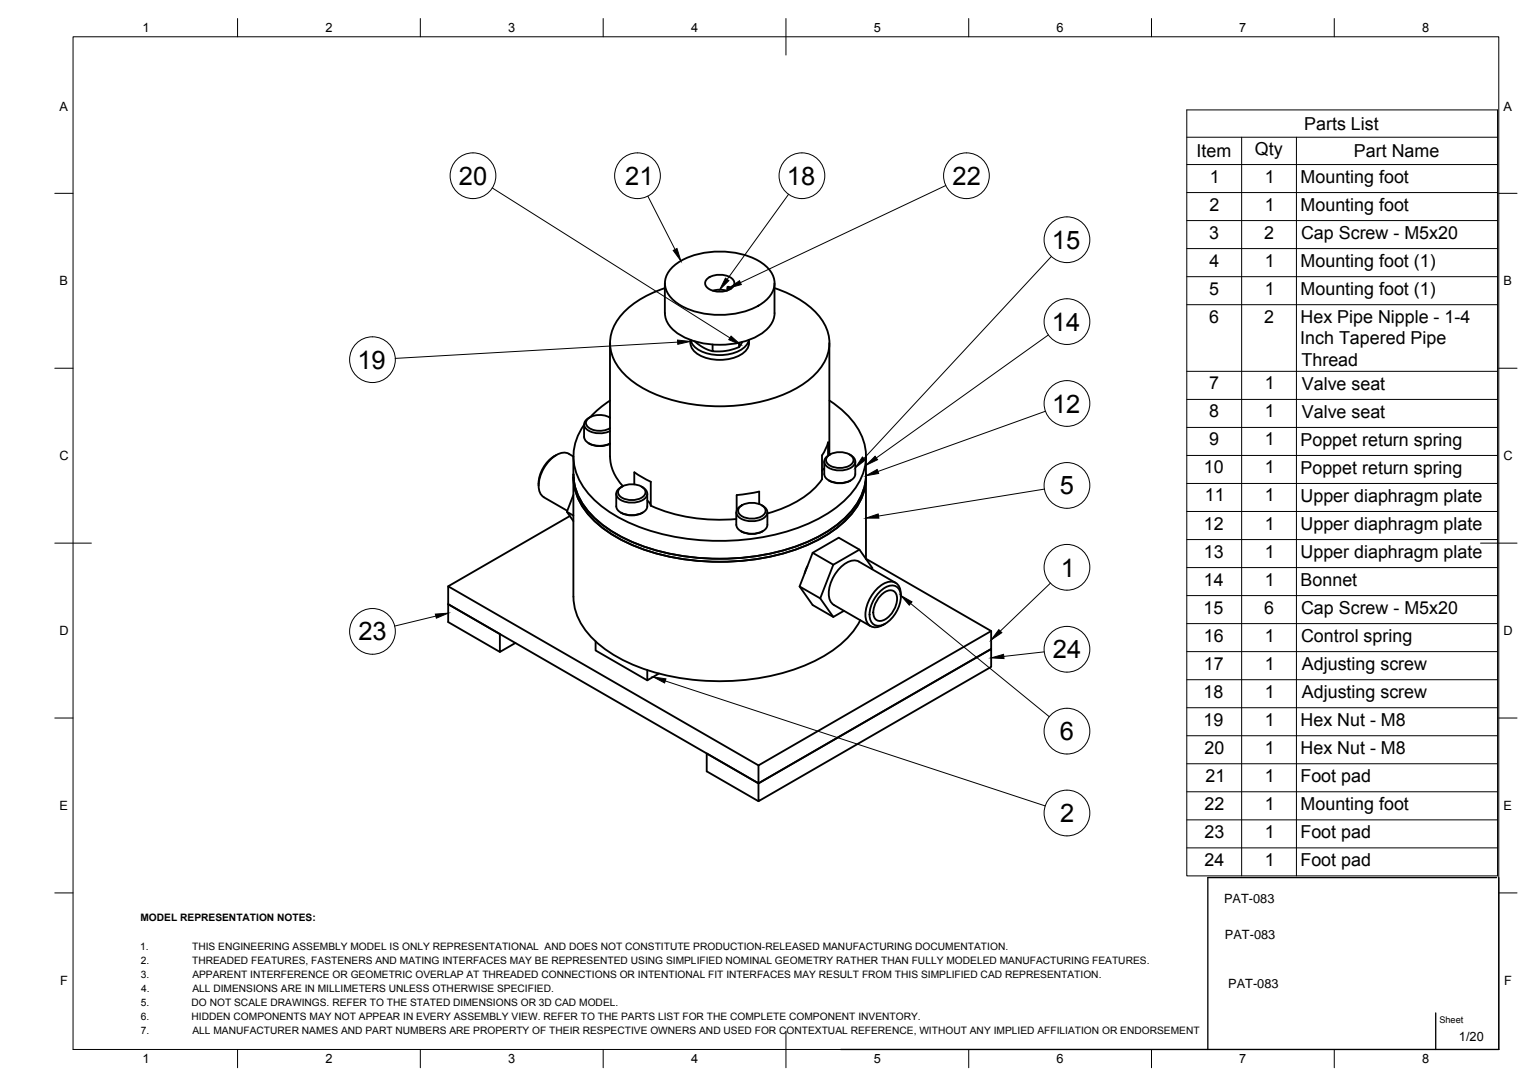
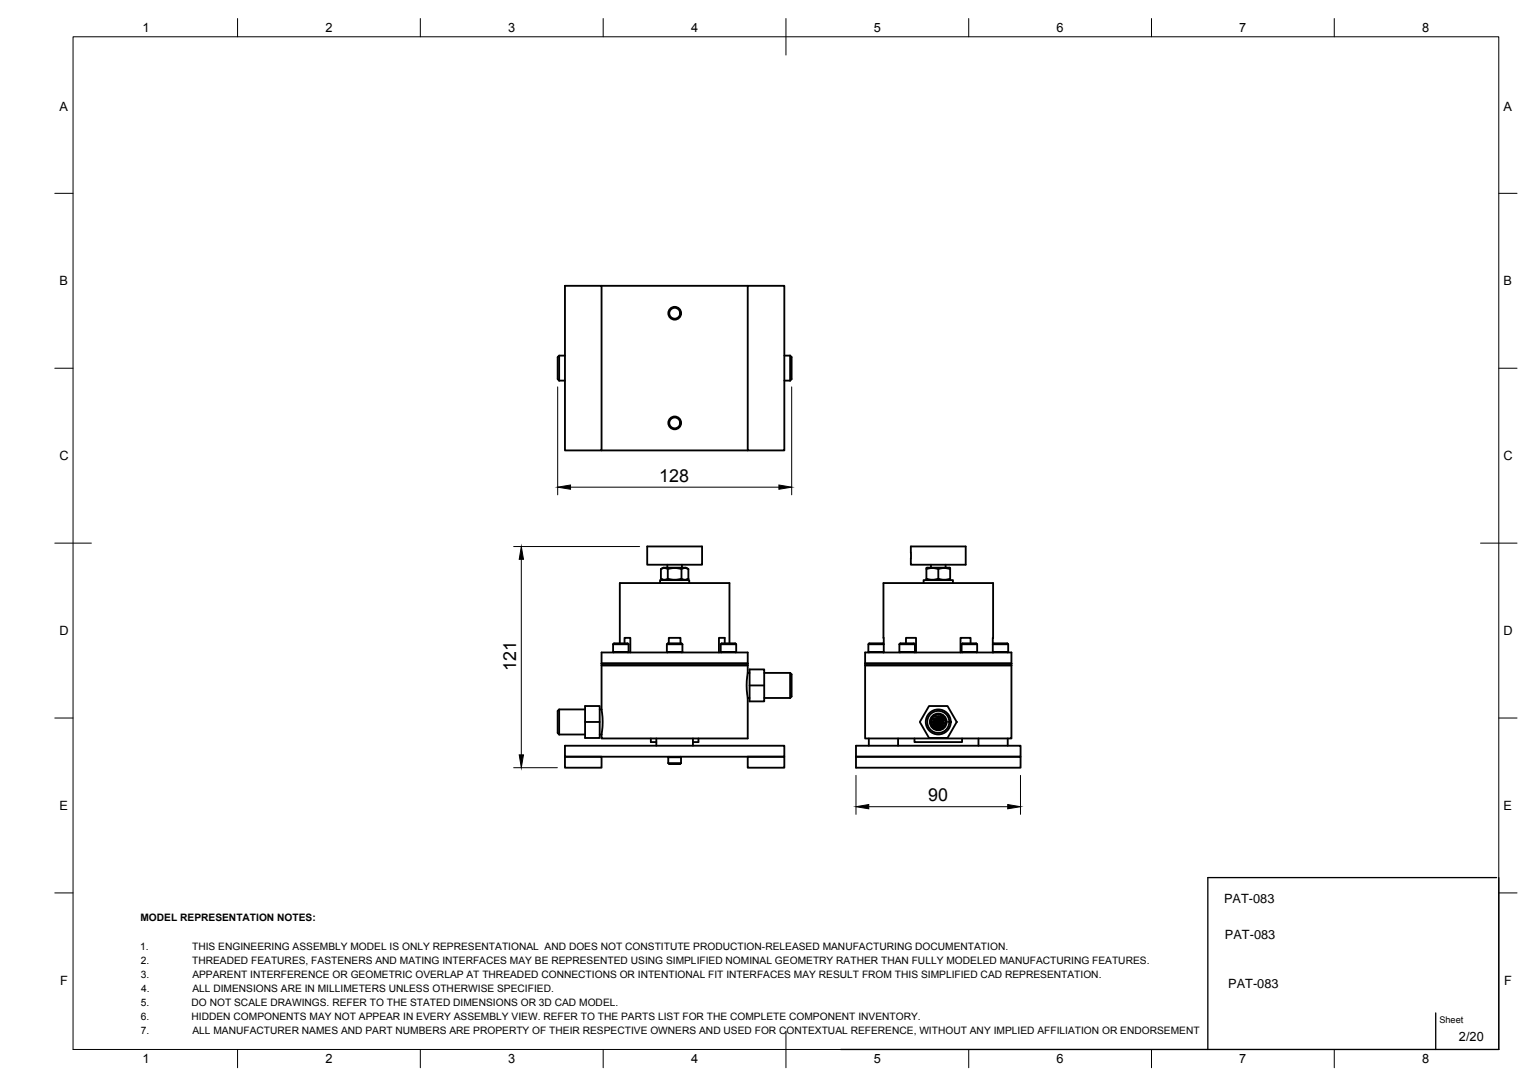
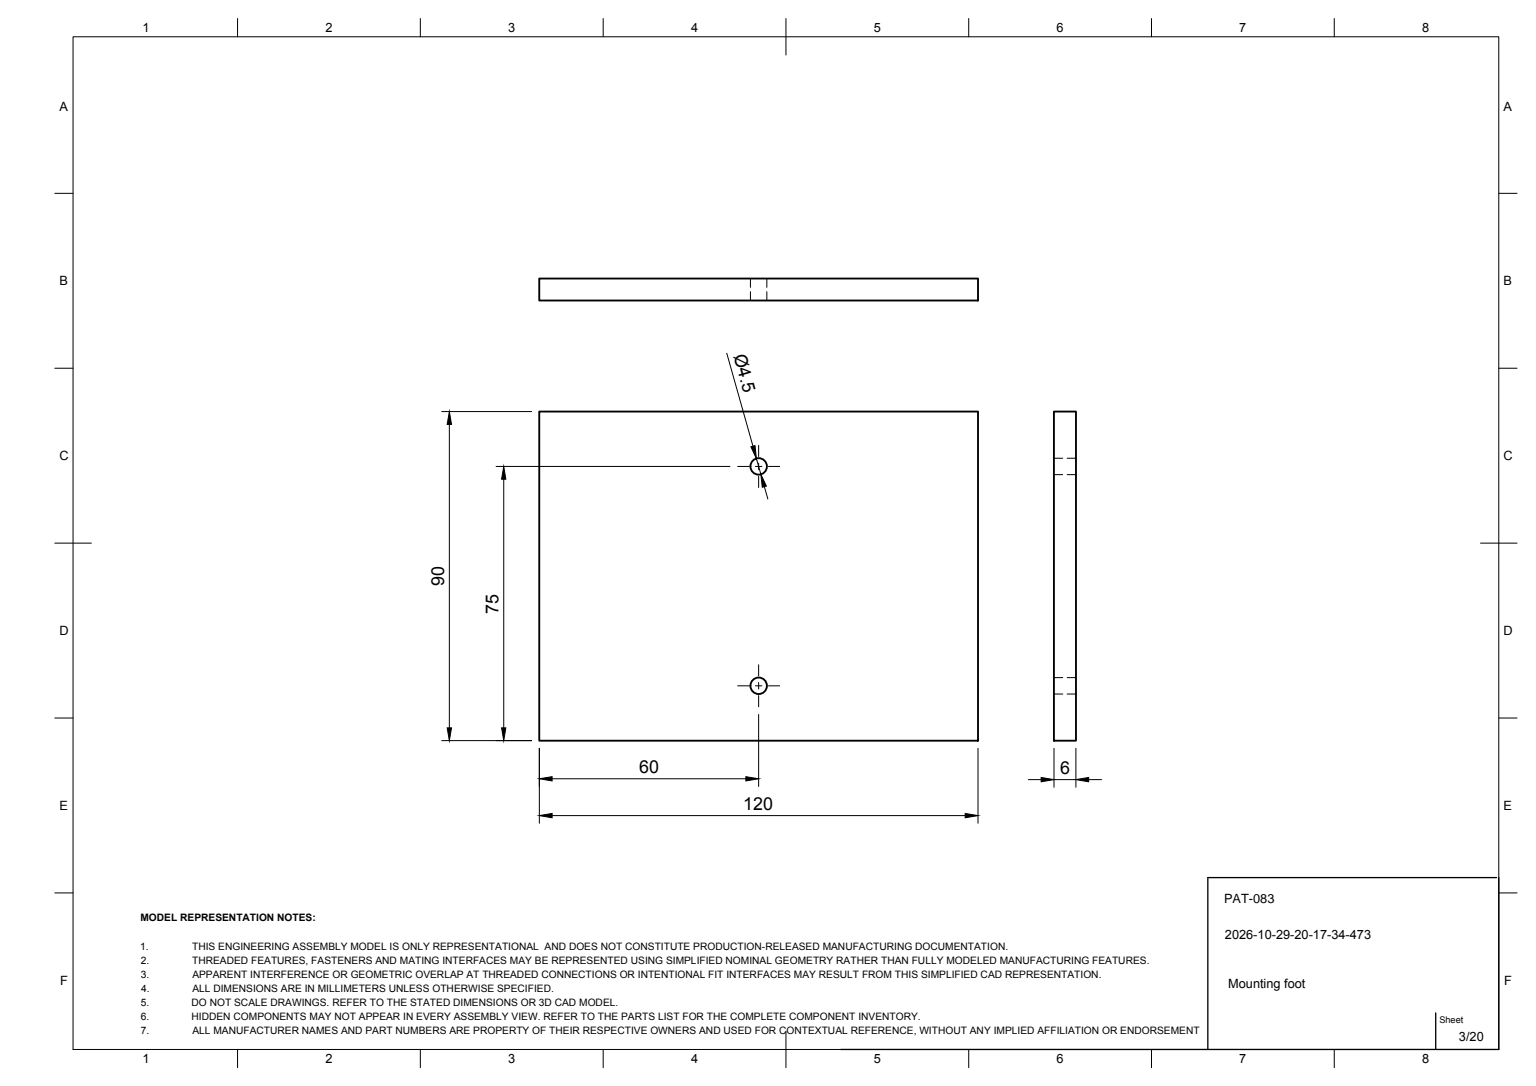
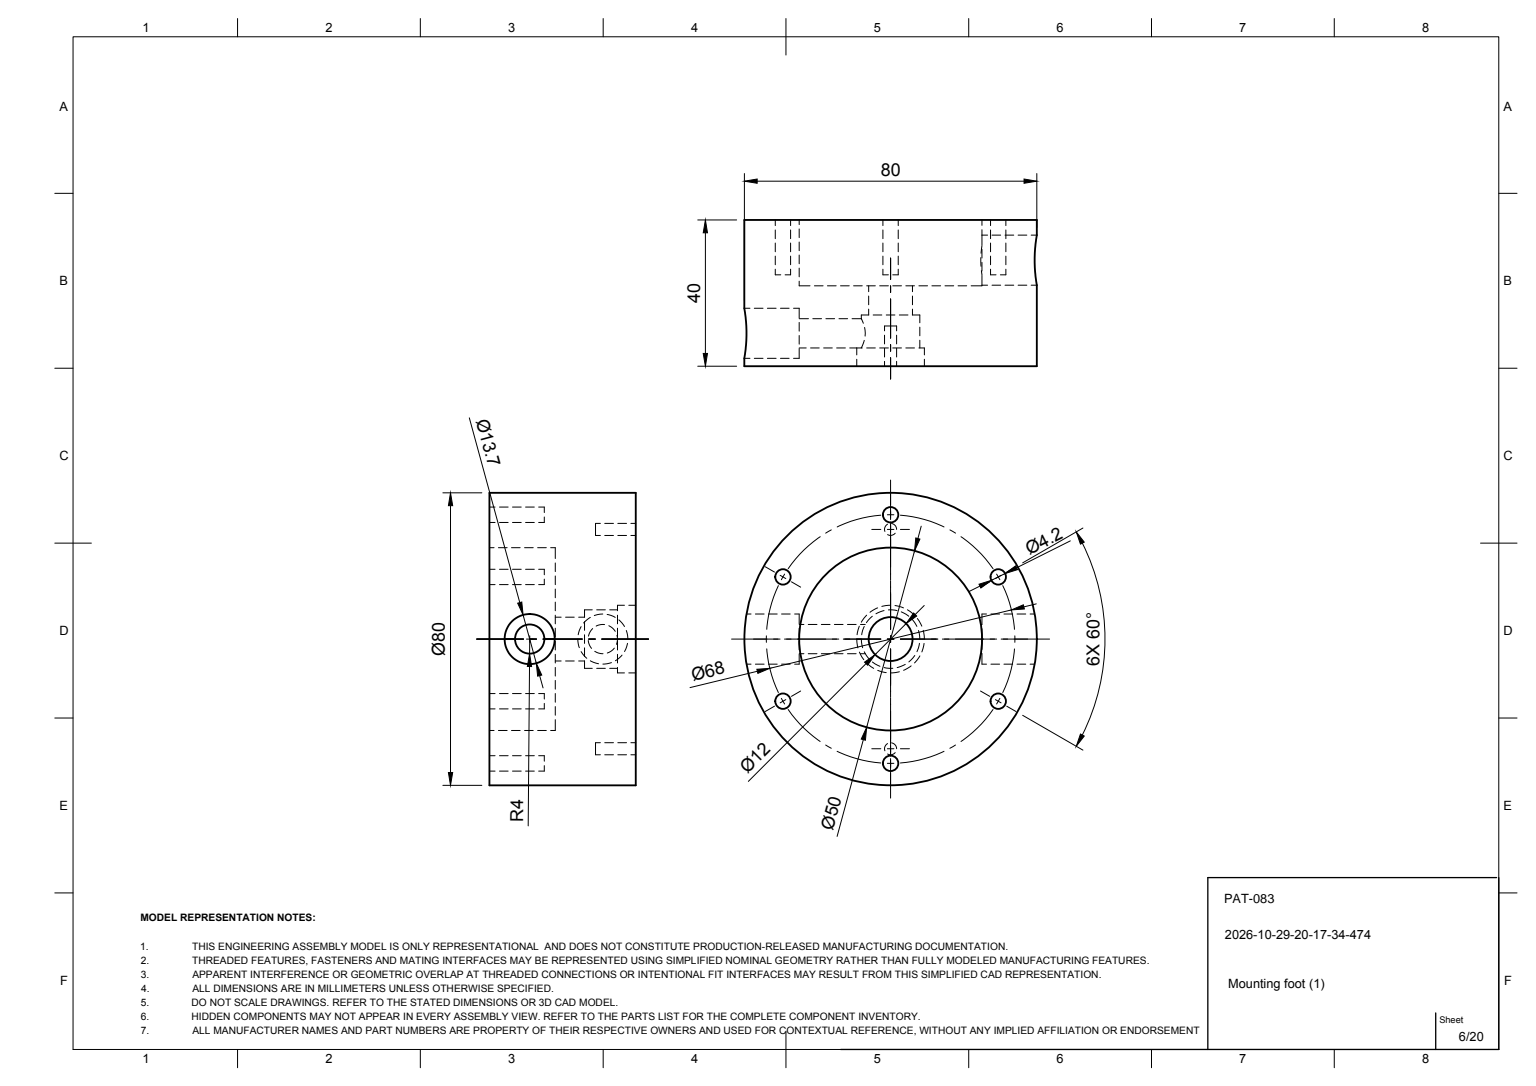
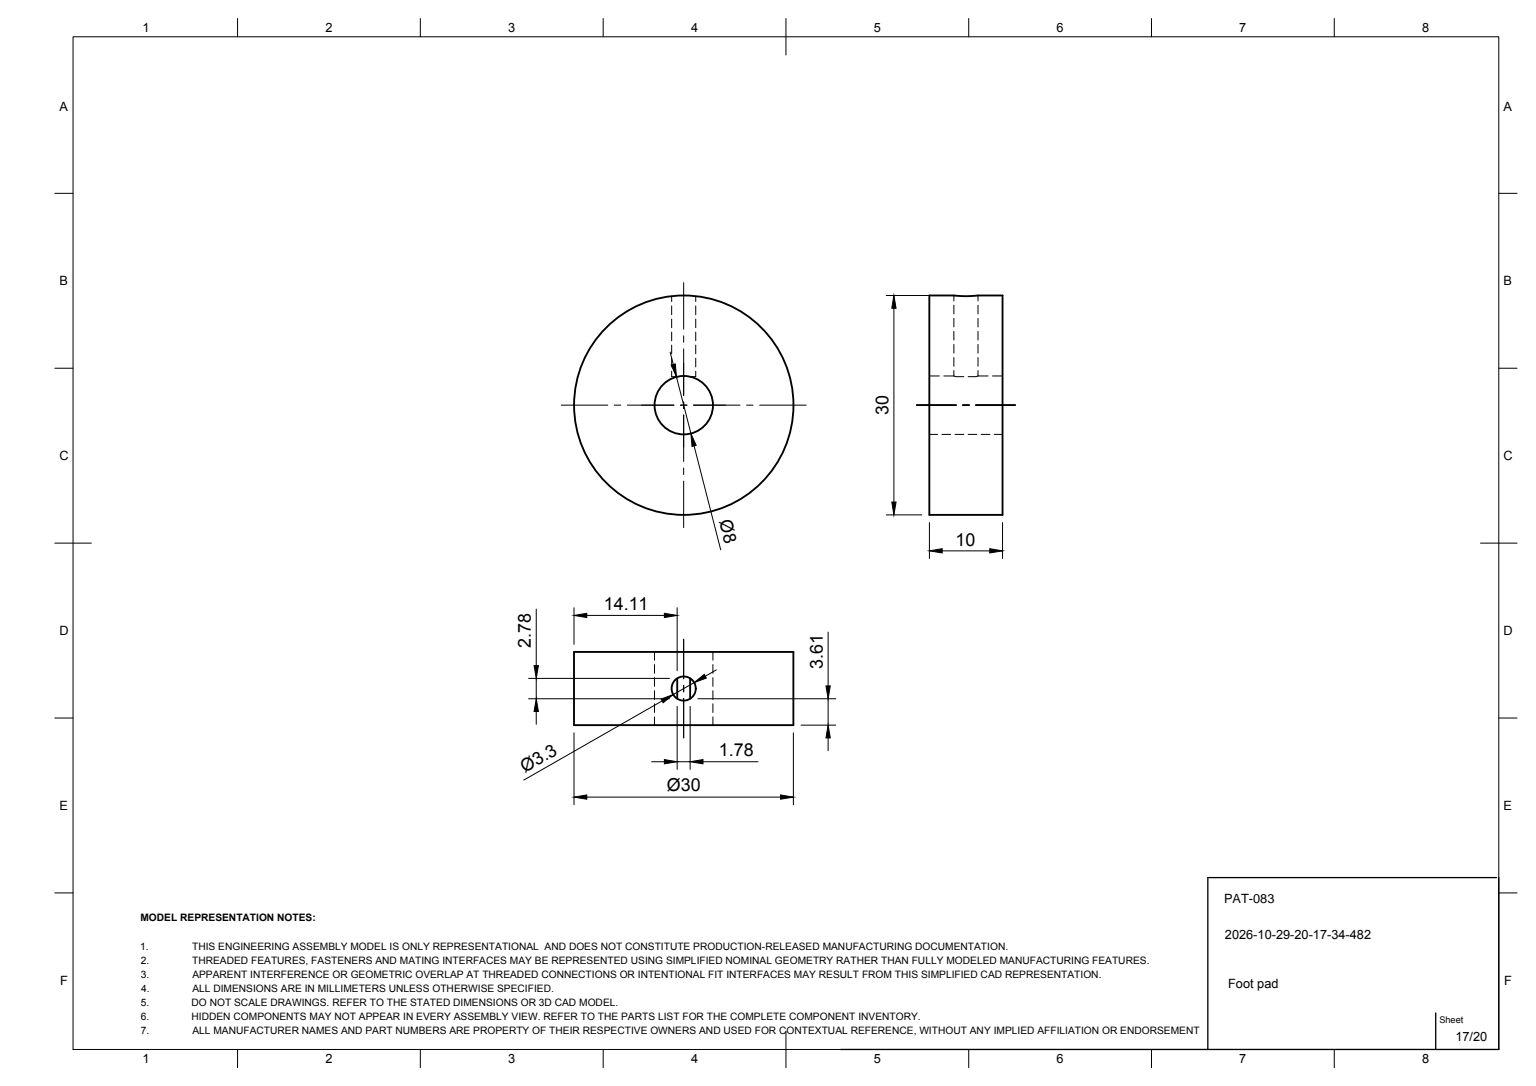
ISO-10303-21;
HEADER;
/* Generated by software containing ST-Developer
 * from STEP Tools, Inc. (www.steptools.com) 
 */

FILE_DESCRIPTION(
/* description */ ('PAT-083'),
/* implementation_level */ '2;1');

FILE_NAME(
/* name */ 'PAT-083',
/* time_stamp */ '2026-10-29T20:18:00-07:00',
/* author */ (''),
/* organization */ (''),
/* preprocessor_version */ 'ST-DEVELOPER v20.2',
/* originating_system */ 'Autodesk Translation Framework v15.17.0.0',
/* authorisation */ '');

FILE_SCHEMA (('AUTOMOTIVE_DESIGN { 1 0 10303 214 3 1 1 }'));
ENDSEC;

DATA;
#10=MECHANICAL_DESIGN_GEOMETRIC_PRESENTATION_REPRESENTATION('',(#229,#230,
#231,#232,#233,#234,#235,#236,#237,#238,#239,#240,#241,#242,#243,#244,#245,
#246,#247,#248,#249,#250,#251,#252),#8428);
#11=ITEM_DEFINED_TRANSFORMATION($,$,#3967,#4405);
#12=ITEM_DEFINED_TRANSFORMATION($,$,#3980,#4406);
#13=ITEM_DEFINED_TRANSFORMATION($,$,#3990,#4407);
#14=ITEM_DEFINED_TRANSFORMATION($,$,#4000,#4408);
#15=ITEM_DEFINED_TRANSFORMATION($,$,#4067,#4409);
#16=ITEM_DEFINED_TRANSFORMATION($,$,#4077,#4410);
#17=ITEM_DEFINED_TRANSFORMATION($,$,#4086,#4411);
#18=ITEM_DEFINED_TRANSFORMATION($,$,#4108,#4412);
#19=ITEM_DEFINED_TRANSFORMATION($,$,#4113,#4413);
#20=ITEM_DEFINED_TRANSFORMATION($,$,#4122,#4414);
#21=ITEM_DEFINED_TRANSFORMATION($,$,#4149,#4415);
#22=ITEM_DEFINED_TRANSFORMATION($,$,#4166,#4416);
#23=ITEM_DEFINED_TRANSFORMATION($,$,#4237,#4417);
#24=ITEM_DEFINED_TRANSFORMATION($,$,#4242,#4418);
#25=ITEM_DEFINED_TRANSFORMATION($,$,#4252,#4419);
#26=ITEM_DEFINED_TRANSFORMATION($,$,#4258,#4420);
#27=ITEM_DEFINED_TRANSFORMATION($,$,#4273,#4421);
#28=ITEM_DEFINED_TRANSFORMATION($,$,#4280,#4422);
#29=ITEM_DEFINED_TRANSFORMATION($,$,#4287,#4423);
#30=ITEM_DEFINED_TRANSFORMATION($,$,#4287,#4424);
#31=ITEM_DEFINED_TRANSFORMATION($,$,#4313,#4425);
#32=ITEM_DEFINED_TRANSFORMATION($,$,#4313,#4426);
#33=ITEM_DEFINED_TRANSFORMATION($,$,#4337,#4427);
#34=ITEM_DEFINED_TRANSFORMATION($,$,#4337,#4428);
#35=ITEM_DEFINED_TRANSFORMATION($,$,#4337,#4429);
#36=ITEM_DEFINED_TRANSFORMATION($,$,#4337,#4430);
#37=ITEM_DEFINED_TRANSFORMATION($,$,#4337,#4431);
#38=ITEM_DEFINED_TRANSFORMATION($,$,#4337,#4432);
#39=ITEM_DEFINED_TRANSFORMATION($,$,#4363,#4433);
#40=ITEM_DEFINED_TRANSFORMATION($,$,#4372,#4434);
#41=ITEM_DEFINED_TRANSFORMATION($,$,#4388,#4435);
#42=(
REPRESENTATION_RELATIONSHIP($,$,#8515,#8514)
REPRESENTATION_RELATIONSHIP_WITH_TRANSFORMATION(#11)
SHAPE_REPRESENTATION_RELATIONSHIP()
);
#43=(
REPRESENTATION_RELATIONSHIP($,$,#8516,#8514)
REPRESENTATION_RELATIONSHIP_WITH_TRANSFORMATION(#12)
SHAPE_REPRESENTATION_RELATIONSHIP()
);
#44=(
REPRESENTATION_RELATIONSHIP($,$,#8517,#8514)
REPRESENTATION_RELATIONSHIP_WITH_TRANSFORMATION(#13)
SHAPE_REPRESENTATION_RELATIONSHIP()
);
#45=(
REPRESENTATION_RELATIONSHIP($,$,#8518,#8514)
REPRESENTATION_RELATIONSHIP_WITH_TRANSFORMATION(#14)
SHAPE_REPRESENTATION_RELATIONSHIP()
);
#46=(
REPRESENTATION_RELATIONSHIP($,$,#8519,#8514)
REPRESENTATION_RELATIONSHIP_WITH_TRANSFORMATION(#15)
SHAPE_REPRESENTATION_RELATIONSHIP()
);
#47=(
REPRESENTATION_RELATIONSHIP($,$,#8520,#8514)
REPRESENTATION_RELATIONSHIP_WITH_TRANSFORMATION(#16)
SHAPE_REPRESENTATION_RELATIONSHIP()
);
#48=(
REPRESENTATION_RELATIONSHIP($,$,#8521,#8514)
REPRESENTATION_RELATIONSHIP_WITH_TRANSFORMATION(#17)
SHAPE_REPRESENTATION_RELATIONSHIP()
);
#49=(
REPRESENTATION_RELATIONSHIP($,$,#8522,#8514)
REPRESENTATION_RELATIONSHIP_WITH_TRANSFORMATION(#18)
SHAPE_REPRESENTATION_RELATIONSHIP()
);
#50=(
REPRESENTATION_RELATIONSHIP($,$,#8523,#8514)
REPRESENTATION_RELATIONSHIP_WITH_TRANSFORMATION(#19)
SHAPE_REPRESENTATION_RELATIONSHIP()
);
#51=(
REPRESENTATION_RELATIONSHIP($,$,#8524,#8514)
REPRESENTATION_RELATIONSHIP_WITH_TRANSFORMATION(#20)
SHAPE_REPRESENTATION_RELATIONSHIP()
);
#52=(
REPRESENTATION_RELATIONSHIP($,$,#8525,#8514)
REPRESENTATION_RELATIONSHIP_WITH_TRANSFORMATION(#21)
SHAPE_REPRESENTATION_RELATIONSHIP()
);
#53=(
REPRESENTATION_RELATIONSHIP($,$,#8526,#8514)
REPRESENTATION_RELATIONSHIP_WITH_TRANSFORMATION(#22)
SHAPE_REPRESENTATION_RELATIONSHIP()
);
#54=(
REPRESENTATION_RELATIONSHIP($,$,#8527,#8514)
REPRESENTATION_RELATIONSHIP_WITH_TRANSFORMATION(#23)
SHAPE_REPRESENTATION_RELATIONSHIP()
);
#55=(
REPRESENTATION_RELATIONSHIP($,$,#8528,#8514)
REPRESENTATION_RELATIONSHIP_WITH_TRANSFORMATION(#24)
SHAPE_REPRESENTATION_RELATIONSHIP()
);
#56=(
REPRESENTATION_RELATIONSHIP($,$,#8529,#8514)
REPRESENTATION_RELATIONSHIP_WITH_TRANSFORMATION(#25)
SHAPE_REPRESENTATION_RELATIONSHIP()
);
#57=(
REPRESENTATION_RELATIONSHIP($,$,#8530,#8514)
REPRESENTATION_RELATIONSHIP_WITH_TRANSFORMATION(#26)
SHAPE_REPRESENTATION_RELATIONSHIP()
);
#58=(
REPRESENTATION_RELATIONSHIP($,$,#8531,#8514)
REPRESENTATION_RELATIONSHIP_WITH_TRANSFORMATION(#27)
SHAPE_REPRESENTATION_RELATIONSHIP()
);
#59=(
REPRESENTATION_RELATIONSHIP($,$,#8532,#8514)
REPRESENTATION_RELATIONSHIP_WITH_TRANSFORMATION(#28)
SHAPE_REPRESENTATION_RELATIONSHIP()
);
#60=(
REPRESENTATION_RELATIONSHIP($,$,#8533,#8514)
REPRESENTATION_RELATIONSHIP_WITH_TRANSFORMATION(#29)
SHAPE_REPRESENTATION_RELATIONSHIP()
);
#61=(
REPRESENTATION_RELATIONSHIP($,$,#8533,#8514)
REPRESENTATION_RELATIONSHIP_WITH_TRANSFORMATION(#30)
SHAPE_REPRESENTATION_RELATIONSHIP()
);
#62=(
REPRESENTATION_RELATIONSHIP($,$,#8534,#8514)
REPRESENTATION_RELATIONSHIP_WITH_TRANSFORMATION(#31)
SHAPE_REPRESENTATION_RELATIONSHIP()
);
#63=(
REPRESENTATION_RELATIONSHIP($,$,#8534,#8514)
REPRESENTATION_RELATIONSHIP_WITH_TRANSFORMATION(#32)
SHAPE_REPRESENTATION_RELATIONSHIP()
);
#64=(
REPRESENTATION_RELATIONSHIP($,$,#8535,#8514)
REPRESENTATION_RELATIONSHIP_WITH_TRANSFORMATION(#33)
SHAPE_REPRESENTATION_RELATIONSHIP()
);
#65=(
REPRESENTATION_RELATIONSHIP($,$,#8535,#8514)
REPRESENTATION_RELATIONSHIP_WITH_TRANSFORMATION(#34)
SHAPE_REPRESENTATION_RELATIONSHIP()
);
#66=(
REPRESENTATION_RELATIONSHIP($,$,#8535,#8514)
REPRESENTATION_RELATIONSHIP_WITH_TRANSFORMATION(#35)
SHAPE_REPRESENTATION_RELATIONSHIP()
);
#67=(
REPRESENTATION_RELATIONSHIP($,$,#8535,#8514)
REPRESENTATION_RELATIONSHIP_WITH_TRANSFORMATION(#36)
SHAPE_REPRESENTATION_RELATIONSHIP()
);
#68=(
REPRESENTATION_RELATIONSHIP($,$,#8535,#8514)
REPRESENTATION_RELATIONSHIP_WITH_TRANSFORMATION(#37)
SHAPE_REPRESENTATION_RELATIONSHIP()
);
#69=(
REPRESENTATION_RELATIONSHIP($,$,#8535,#8514)
REPRESENTATION_RELATIONSHIP_WITH_TRANSFORMATION(#38)
SHAPE_REPRESENTATION_RELATIONSHIP()
);
#70=(
REPRESENTATION_RELATIONSHIP($,$,#8536,#8514)
REPRESENTATION_RELATIONSHIP_WITH_TRANSFORMATION(#39)
SHAPE_REPRESENTATION_RELATIONSHIP()
);
#71=(
REPRESENTATION_RELATIONSHIP($,$,#8537,#8514)
REPRESENTATION_RELATIONSHIP_WITH_TRANSFORMATION(#40)
SHAPE_REPRESENTATION_RELATIONSHIP()
);
#72=(
REPRESENTATION_RELATIONSHIP($,$,#8538,#8514)
REPRESENTATION_RELATIONSHIP_WITH_TRANSFORMATION(#41)
SHAPE_REPRESENTATION_RELATIONSHIP()
);
#73=CONTEXT_DEPENDENT_SHAPE_REPRESENTATION(#42,#8483);
#74=CONTEXT_DEPENDENT_SHAPE_REPRESENTATION(#43,#8484);
#75=CONTEXT_DEPENDENT_SHAPE_REPRESENTATION(#44,#8485);
#76=CONTEXT_DEPENDENT_SHAPE_REPRESENTATION(#45,#8486);
#77=CONTEXT_DEPENDENT_SHAPE_REPRESENTATION(#46,#8487);
#78=CONTEXT_DEPENDENT_SHAPE_REPRESENTATION(#47,#8488);
#79=CONTEXT_DEPENDENT_SHAPE_REPRESENTATION(#48,#8489);
#80=CONTEXT_DEPENDENT_SHAPE_REPRESENTATION(#49,#8490);
#81=CONTEXT_DEPENDENT_SHAPE_REPRESENTATION(#50,#8491);
#82=CONTEXT_DEPENDENT_SHAPE_REPRESENTATION(#51,#8492);
#83=CONTEXT_DEPENDENT_SHAPE_REPRESENTATION(#52,#8493);
#84=CONTEXT_DEPENDENT_SHAPE_REPRESENTATION(#53,#8494);
#85=CONTEXT_DEPENDENT_SHAPE_REPRESENTATION(#54,#8495);
#86=CONTEXT_DEPENDENT_SHAPE_REPRESENTATION(#55,#8496);
#87=CONTEXT_DEPENDENT_SHAPE_REPRESENTATION(#56,#8497);
#88=CONTEXT_DEPENDENT_SHAPE_REPRESENTATION(#57,#8498);
#89=CONTEXT_DEPENDENT_SHAPE_REPRESENTATION(#58,#8499);
#90=CONTEXT_DEPENDENT_SHAPE_REPRESENTATION(#59,#8500);
#91=CONTEXT_DEPENDENT_SHAPE_REPRESENTATION(#60,#8501);
#92=CONTEXT_DEPENDENT_SHAPE_REPRESENTATION(#61,#8502);
#93=CONTEXT_DEPENDENT_SHAPE_REPRESENTATION(#62,#8503);
#94=CONTEXT_DEPENDENT_SHAPE_REPRESENTATION(#63,#8504);
#95=CONTEXT_DEPENDENT_SHAPE_REPRESENTATION(#64,#8505);
#96=CONTEXT_DEPENDENT_SHAPE_REPRESENTATION(#65,#8506);
#97=CONTEXT_DEPENDENT_SHAPE_REPRESENTATION(#66,#8507);
#98=CONTEXT_DEPENDENT_SHAPE_REPRESENTATION(#67,#8508);
#99=CONTEXT_DEPENDENT_SHAPE_REPRESENTATION(#68,#8509);
#100=CONTEXT_DEPENDENT_SHAPE_REPRESENTATION(#69,#8510);
#101=CONTEXT_DEPENDENT_SHAPE_REPRESENTATION(#70,#8511);
#102=CONTEXT_DEPENDENT_SHAPE_REPRESENTATION(#71,#8512);
#103=CONTEXT_DEPENDENT_SHAPE_REPRESENTATION(#72,#8513);
#104=NEXT_ASSEMBLY_USAGE_OCCURRENCE('Base:1','Base:1','Base:1',#8540,#8541,
'Base:1');
#105=NEXT_ASSEMBLY_USAGE_OCCURRENCE('Mounting foot:1','Mounting foot:1',
'Mounting foot:1',#8540,#8542,'Mounting foot:1');
#106=NEXT_ASSEMBLY_USAGE_OCCURRENCE('Mounting foot (1):1',
'Mounting foot (1):1','Mounting foot (1):1',#8540,#8543,
'Mounting foot (1):1');
#107=NEXT_ASSEMBLY_USAGE_OCCURRENCE('Lower body:1','Lower body:1',
'Lower body:1',#8540,#8544,'Lower body:1');
#108=NEXT_ASSEMBLY_USAGE_OCCURRENCE('Bottom service plug:1',
'Bottom service plug:1','Bottom service plug:1',#8540,#8545,
'Bottom service plug:1');
#109=NEXT_ASSEMBLY_USAGE_OCCURRENCE('Valve seat:1','Valve seat:1',
'Valve seat:1',#8540,#8546,'Valve seat:1');
#110=NEXT_ASSEMBLY_USAGE_OCCURRENCE('Poppet and stem:1',
'Poppet and stem:1','Poppet and stem:1',#8540,#8547,'Poppet and stem:1');
#111=NEXT_ASSEMBLY_USAGE_OCCURRENCE('Poppet return spring:1',
'Poppet return spring:1','Poppet return spring:1',#8540,#8548,
'Poppet return spring:1');
#112=NEXT_ASSEMBLY_USAGE_OCCURRENCE('Lower diaphragm plate:1',
'Lower diaphragm plate:1','Lower diaphragm plate:1',#8540,#8549,
'Lower diaphragm plate:1');
#113=NEXT_ASSEMBLY_USAGE_OCCURRENCE('Diaphragm:1','Diaphragm:1',
'Diaphragm:1',#8540,#8550,'Diaphragm:1');
#114=NEXT_ASSEMBLY_USAGE_OCCURRENCE('Upper diaphragm plate:1',
'Upper diaphragm plate:1','Upper diaphragm plate:1',#8540,#8551,
'Upper diaphragm plate:1');
#115=NEXT_ASSEMBLY_USAGE_OCCURRENCE('Bonnet:1','Bonnet:1','Bonnet:1',#8540,
#8552,'Bonnet:1');
#116=NEXT_ASSEMBLY_USAGE_OCCURRENCE('Control spring:1',
'Control spring:1','Control spring:1',#8540,#8553,'Control spring:1');
#117=NEXT_ASSEMBLY_USAGE_OCCURRENCE('Adjuster spring shoe:1',
'Adjuster spring shoe:1','Adjuster spring shoe:1',#8540,#8554,
'Adjuster spring shoe:1');
#118=NEXT_ASSEMBLY_USAGE_OCCURRENCE('Adjusting screw:1',
'Adjusting screw:1','Adjusting screw:1',#8540,#8555,'Adjusting screw:1');
#119=NEXT_ASSEMBLY_USAGE_OCCURRENCE('Adjuster knob:1','Adjuster knob:1',
'Adjuster knob:1',#8540,#8556,'Adjuster knob:1');
#120=NEXT_ASSEMBLY_USAGE_OCCURRENCE('Foot pad:1','Foot pad:1',
'Foot pad:1',#8540,#8557,'Foot pad:1');
#121=NEXT_ASSEMBLY_USAGE_OCCURRENCE('Foot pad (1):1','Foot pad (1):1',
'Foot pad (1):1',#8540,#8558,'Foot pad (1):1');
#122=NEXT_ASSEMBLY_USAGE_OCCURRENCE('Cap Screw - M4x16:1',
'Cap Screw - M4x16:1','Cap Screw - M4x16:1',#8540,#8559,
'Cap Screw - M4x16:1');
#123=NEXT_ASSEMBLY_USAGE_OCCURRENCE('Cap Screw - M4x16:2',
'Cap Screw - M4x16:2','Cap Screw - M4x16:2',#8540,#8559,
'Cap Screw - M4x16:2');
#124=NEXT_ASSEMBLY_USAGE_OCCURRENCE(
'Hex Pipe Nipple - 1-4 Inch Tapered Pipe Thread:1',
'Hex Pipe Nipple - 1-4 Inch Tapered Pipe Thread:1',
'Hex Pipe Nipple - 1-4 Inch Tapered Pipe Thread:1',#8540,#8560,
'Hex Pipe Nipple - 1-4 Inch Tapered Pipe Thread:1');
#125=NEXT_ASSEMBLY_USAGE_OCCURRENCE(
'Hex Pipe Nipple - 1-4 Inch Tapered Pipe Thread:2',
'Hex Pipe Nipple - 1-4 Inch Tapered Pipe Thread:2',
'Hex Pipe Nipple - 1-4 Inch Tapered Pipe Thread:2',#8540,#8560,
'Hex Pipe Nipple - 1-4 Inch Tapered Pipe Thread:2');
#126=NEXT_ASSEMBLY_USAGE_OCCURRENCE('Cap Screw - M5x20:1',
'Cap Screw - M5x20:1','Cap Screw - M5x20:1',#8540,#8561,
'Cap Screw - M5x20:1');
#127=NEXT_ASSEMBLY_USAGE_OCCURRENCE('Cap Screw - M5x20:2',
'Cap Screw - M5x20:2','Cap Screw - M5x20:2',#8540,#8561,
'Cap Screw - M5x20:2');
#128=NEXT_ASSEMBLY_USAGE_OCCURRENCE('Cap Screw - M5x20:3',
'Cap Screw - M5x20:3','Cap Screw - M5x20:3',#8540,#8561,
'Cap Screw - M5x20:3');
#129=NEXT_ASSEMBLY_USAGE_OCCURRENCE('Cap Screw - M5x20:4',
'Cap Screw - M5x20:4','Cap Screw - M5x20:4',#8540,#8561,
'Cap Screw - M5x20:4');
#130=NEXT_ASSEMBLY_USAGE_OCCURRENCE('Cap Screw - M5x20:5',
'Cap Screw - M5x20:5','Cap Screw - M5x20:5',#8540,#8561,
'Cap Screw - M5x20:5');
#131=NEXT_ASSEMBLY_USAGE_OCCURRENCE('Cap Screw - M5x20:6',
'Cap Screw - M5x20:6','Cap Screw - M5x20:6',#8540,#8561,
'Cap Screw - M5x20:6');
#132=NEXT_ASSEMBLY_USAGE_OCCURRENCE('Flat Washer - M8:1',
'Flat Washer - M8:1','Flat Washer - M8:1',#8540,#8562,
'Flat Washer - M8:1');
#133=NEXT_ASSEMBLY_USAGE_OCCURRENCE('Hex Nut - M8:1','Hex Nut - M8:1',
'Hex Nut - M8:1',#8540,#8563,'Hex Nut - M8:1');
#134=NEXT_ASSEMBLY_USAGE_OCCURRENCE('Socket Set Screw - M4x6:1',
'Socket Set Screw - M4x6:1','Socket Set Screw - M4x6:1',#8540,#8564,
'Socket Set Screw - M4x6:1');
#135=(
BOUNDED_CURVE()
B_SPLINE_CURVE(2,(#8219,#8220,#8221),.UNSPECIFIED.,.F.,.F.)
B_SPLINE_CURVE_WITH_KNOTS((3,3),(0.14973948338295,0.97160236658079),
 .UNSPECIFIED.)
CURVE()
GEOMETRIC_REPRESENTATION_ITEM()
RATIONAL_B_SPLINE_CURVE((1.07140024848292,1.23714644374248,1.07140024848292))
REPRESENTATION_ITEM('')
);
#136=(
BOUNDED_CURVE()
B_SPLINE_CURVE(2,(#8223,#8224,#8225),.UNSPECIFIED.,.F.,.F.)
B_SPLINE_CURVE_WITH_KNOTS((3,3),(0.14973948338295,0.971602366580789),
 .UNSPECIFIED.)
CURVE()
GEOMETRIC_REPRESENTATION_ITEM()
RATIONAL_B_SPLINE_CURVE((1.07140024848292,1.23714644374248,1.07140024848292))
REPRESENTATION_ITEM('')
);
#137=(
BOUNDED_CURVE()
B_SPLINE_CURVE(2,(#8230,#8231,#8232),.UNSPECIFIED.,.F.,.F.)
B_SPLINE_CURVE_WITH_KNOTS((3,3),(0.14973948338295,0.97160236658079),
 .UNSPECIFIED.)
CURVE()
GEOMETRIC_REPRESENTATION_ITEM()
RATIONAL_B_SPLINE_CURVE((1.07140024848292,1.23714644374248,1.07140024848292))
REPRESENTATION_ITEM('')
);
#138=(
BOUNDED_CURVE()
B_SPLINE_CURVE(2,(#8234,#8235,#8236),.UNSPECIFIED.,.F.,.F.)
B_SPLINE_CURVE_WITH_KNOTS((3,3),(0.14973948338295,0.97160236658079),
 .UNSPECIFIED.)
CURVE()
GEOMETRIC_REPRESENTATION_ITEM()
RATIONAL_B_SPLINE_CURVE((1.07140024848292,1.23714644374248,1.07140024848292))
REPRESENTATION_ITEM('')
);
#139=(
BOUNDED_CURVE()
B_SPLINE_CURVE(2,(#8238,#8239,#8240),.UNSPECIFIED.,.F.,.F.)
B_SPLINE_CURVE_WITH_KNOTS((3,3),(0.14973948338295,0.971602366580789),
 .UNSPECIFIED.)
CURVE()
GEOMETRIC_REPRESENTATION_ITEM()
RATIONAL_B_SPLINE_CURVE((1.07140024848292,1.23714644374248,1.07140024848292))
REPRESENTATION_ITEM('')
);
#140=(
BOUNDED_CURVE()
B_SPLINE_CURVE(2,(#8241,#8242,#8243),.UNSPECIFIED.,.F.,.F.)
B_SPLINE_CURVE_WITH_KNOTS((3,3),(0.14973948338295,0.97160236658079),
 .UNSPECIFIED.)
CURVE()
GEOMETRIC_REPRESENTATION_ITEM()
RATIONAL_B_SPLINE_CURVE((1.07140024848292,1.23714644374248,1.07140024848292))
REPRESENTATION_ITEM('')
);
#141=(
BOUNDED_CURVE()
B_SPLINE_CURVE(2,(#8250,#8251,#8252),.UNSPECIFIED.,.F.,.F.)
B_SPLINE_CURVE_WITH_KNOTS((3,3),(0.14973948338295,0.97160236658079),
 .UNSPECIFIED.)
CURVE()
GEOMETRIC_REPRESENTATION_ITEM()
RATIONAL_B_SPLINE_CURVE((1.07140024848292,1.23714644374248,1.07140024848292))
REPRESENTATION_ITEM('')
);
#142=(
BOUNDED_CURVE()
B_SPLINE_CURVE(2,(#8254,#8255,#8256),.UNSPECIFIED.,.F.,.F.)
B_SPLINE_CURVE_WITH_KNOTS((3,3),(0.14973948338295,0.97160236658079),
 .UNSPECIFIED.)
CURVE()
GEOMETRIC_REPRESENTATION_ITEM()
RATIONAL_B_SPLINE_CURVE((1.07140024848292,1.23714644374248,1.07140024848292))
REPRESENTATION_ITEM('')
);
#143=(
BOUNDED_CURVE()
B_SPLINE_CURVE(2,(#8258,#8259,#8260),.UNSPECIFIED.,.F.,.F.)
B_SPLINE_CURVE_WITH_KNOTS((3,3),(0.14973948338295,0.971602366580789),
 .UNSPECIFIED.)
CURVE()
GEOMETRIC_REPRESENTATION_ITEM()
RATIONAL_B_SPLINE_CURVE((1.07140024848292,1.23714644374248,1.07140024848292))
REPRESENTATION_ITEM('')
);
#144=(
BOUNDED_CURVE()
B_SPLINE_CURVE(2,(#8262,#8263,#8264),.UNSPECIFIED.,.F.,.F.)
B_SPLINE_CURVE_WITH_KNOTS((3,3),(0.14973948338295,0.97160236658079),
 .UNSPECIFIED.)
CURVE()
GEOMETRIC_REPRESENTATION_ITEM()
RATIONAL_B_SPLINE_CURVE((1.07140024848292,1.23714644374248,1.07140024848292))
REPRESENTATION_ITEM('')
);
#145=(
BOUNDED_CURVE()
B_SPLINE_CURVE(2,(#8266,#8267,#8268),.UNSPECIFIED.,.F.,.F.)
B_SPLINE_CURVE_WITH_KNOTS((3,3),(0.14973948338295,0.97160236658079),
 .UNSPECIFIED.)
CURVE()
GEOMETRIC_REPRESENTATION_ITEM()
RATIONAL_B_SPLINE_CURVE((1.07140024848292,1.23714644374248,1.07140024848292))
REPRESENTATION_ITEM('')
);
#146=(
BOUNDED_CURVE()
B_SPLINE_CURVE(2,(#8269,#8270,#8271),.UNSPECIFIED.,.F.,.F.)
B_SPLINE_CURVE_WITH_KNOTS((3,3),(0.14973948338295,0.971602366580789),
 .UNSPECIFIED.)
CURVE()
GEOMETRIC_REPRESENTATION_ITEM()
RATIONAL_B_SPLINE_CURVE((1.07140024848292,1.23714644374248,1.07140024848292))
REPRESENTATION_ITEM('')
);
#147=ORIENTED_CLOSED_SHELL('',*,#3694,.F.);
#148=ORIENTED_CLOSED_SHELL('',*,#3697,.F.);
#149=CONICAL_SURFACE('',#4290,0.325,0.785398163397448);
#150=CONICAL_SURFACE('',#4294,0.335,0.785398163397448);
#151=CONICAL_SURFACE('',#4298,0.21,0.463647609000806);
#152=CONICAL_SURFACE('',#4302,0.18,0.785398163397448);
#153=CONICAL_SURFACE('',#4329,0.645,0.785398163397448);
#154=CONICAL_SURFACE('',#4332,0.645,0.785398163397448);
#155=CONICAL_SURFACE('',#4340,0.4,0.785398163397448);
#156=CONICAL_SURFACE('',#4344,0.41,0.785398163397448);
#157=CONICAL_SURFACE('',#4348,0.26,0.463647609000806);
#158=CONICAL_SURFACE('',#4352,0.225,0.785398163397448);
#159=CONICAL_SURFACE('',#4373,0.734027674973257,1.0471975511966);
#160=CONICAL_SURFACE('',#4375,0.734027674973257,1.0471975511966);
#161=CONICAL_SURFACE('',#4398,0.185,0.785398163397449);
#162=CONICAL_SURFACE('',#4402,0.1625,0.785398163397449);
#163=BREP_WITH_VOIDS('Body1',#3693,(#147));
#164=BREP_WITH_VOIDS('Body1',#3696,(#148));
#165=B_SPLINE_SURFACE_WITH_KNOTS('',3,3,((#6072,#6073,#6074,#6075,#6076,
#6077,#6078,#6079,#6080,#6081,#6082,#6083,#6084,#6085,#6086,#6087,#6088,
#6089,#6090,#6091,#6092,#6093,#6094,#6095,#6096,#6097,#6098,#6099,#6100,
#6101,#6102,#6103,#6104,#6105,#6106,#6107,#6108,#6109,#6110,#6111,#6112,
#6113,#6114,#6115,#6116,#6117,#6118,#6119,#6120,#6121,#6122,#6123,#6124,
#6125,#6126,#6127,#6128,#6129,#6130,#6131,#6132),(#6133,#6134,#6135,#6136,
#6137,#6138,#6139,#6140,#6141,#6142,#6143,#6144,#6145,#6146,#6147,#6148,
#6149,#6150,#6151,#6152,#6153,#6154,#6155,#6156,#6157,#6158,#6159,#6160,
#6161,#6162,#6163,#6164,#6165,#6166,#6167,#6168,#6169,#6170,#6171,#6172,
#6173,#6174,#6175,#6176,#6177,#6178,#6179,#6180,#6181,#6182,#6183,#6184,
#6185,#6186,#6187,#6188,#6189,#6190,#6191,#6192,#6193),(#6194,#6195,#6196,
#6197,#6198,#6199,#6200,#6201,#6202,#6203,#6204,#6205,#6206,#6207,#6208,
#6209,#6210,#6211,#6212,#6213,#6214,#6215,#6216,#6217,#6218,#6219,#6220,
#6221,#6222,#6223,#6224,#6225,#6226,#6227,#6228,#6229,#6230,#6231,#6232,
#6233,#6234,#6235,#6236,#6237,#6238,#6239,#6240,#6241,#6242,#6243,#6244,
#6245,#6246,#6247,#6248,#6249,#6250,#6251,#6252,#6253,#6254),(#6255,#6256,
#6257,#6258,#6259,#6260,#6261,#6262,#6263,#6264,#6265,#6266,#6267,#6268,
#6269,#6270,#6271,#6272,#6273,#6274,#6275,#6276,#6277,#6278,#6279,#6280,
#6281,#6282,#6283,#6284,#6285,#6286,#6287,#6288,#6289,#6290,#6291,#6292,
#6293,#6294,#6295,#6296,#6297,#6298,#6299,#6300,#6301,#6302,#6303,#6304,
#6305,#6306,#6307,#6308,#6309,#6310,#6311,#6312,#6313,#6314,#6315),(#6316,
#6317,#6318,#6319,#6320,#6321,#6322,#6323,#6324,#6325,#6326,#6327,#6328,
#6329,#6330,#6331,#6332,#6333,#6334,#6335,#6336,#6337,#6338,#6339,#6340,
#6341,#6342,#6343,#6344,#6345,#6346,#6347,#6348,#6349,#6350,#6351,#6352,
#6353,#6354,#6355,#6356,#6357,#6358,#6359,#6360,#6361,#6362,#6363,#6364,
#6365,#6366,#6367,#6368,#6369,#6370,#6371,#6372,#6373,#6374,#6375,#6376),
(#6377,#6378,#6379,#6380,#6381,#6382,#6383,#6384,#6385,#6386,#6387,#6388,
#6389,#6390,#6391,#6392,#6393,#6394,#6395,#6396,#6397,#6398,#6399,#6400,
#6401,#6402,#6403,#6404,#6405,#6406,#6407,#6408,#6409,#6410,#6411,#6412,
#6413,#6414,#6415,#6416,#6417,#6418,#6419,#6420,#6421,#6422,#6423,#6424,
#6425,#6426,#6427,#6428,#6429,#6430,#6431,#6432,#6433,#6434,#6435,#6436,
#6437),(#6438,#6439,#6440,#6441,#6442,#6443,#6444,#6445,#6446,#6447,#6448,
#6449,#6450,#6451,#6452,#6453,#6454,#6455,#6456,#6457,#6458,#6459,#6460,
#6461,#6462,#6463,#6464,#6465,#6466,#6467,#6468,#6469,#6470,#6471,#6472,
#6473,#6474,#6475,#6476,#6477,#6478,#6479,#6480,#6481,#6482,#6483,#6484,
#6485,#6486,#6487,#6488,#6489,#6490,#6491,#6492,#6493,#6494,#6495,#6496,
#6497,#6498),(#6499,#6500,#6501,#6502,#6503,#6504,#6505,#6506,#6507,#6508,
#6509,#6510,#6511,#6512,#6513,#6514,#6515,#6516,#6517,#6518,#6519,#6520,
#6521,#6522,#6523,#6524,#6525,#6526,#6527,#6528,#6529,#6530,#6531,#6532,
#6533,#6534,#6535,#6536,#6537,#6538,#6539,#6540,#6541,#6542,#6543,#6544,
#6545,#6546,#6547,#6548,#6549,#6550,#6551,#6552,#6553,#6554,#6555,#6556,
#6557,#6558,#6559),(#6560,#6561,#6562,#6563,#6564,#6565,#6566,#6567,#6568,
#6569,#6570,#6571,#6572,#6573,#6574,#6575,#6576,#6577,#6578,#6579,#6580,
#6581,#6582,#6583,#6584,#6585,#6586,#6587,#6588,#6589,#6590,#6591,#6592,
#6593,#6594,#6595,#6596,#6597,#6598,#6599,#6600,#6601,#6602,#6603,#6604,
#6605,#6606,#6607,#6608,#6609,#6610,#6611,#6612,#6613,#6614,#6615,#6616,
#6617,#6618,#6619,#6620),(#6621,#6622,#6623,#6624,#6625,#6626,#6627,#6628,
#6629,#6630,#6631,#6632,#6633,#6634,#6635,#6636,#6637,#6638,#6639,#6640,
#6641,#6642,#6643,#6644,#6645,#6646,#6647,#6648,#6649,#6650,#6651,#6652,
#6653,#6654,#6655,#6656,#6657,#6658,#6659,#6660,#6661,#6662,#6663,#6664,
#6665,#6666,#6667,#6668,#6669,#6670,#6671,#6672,#6673,#6674,#6675,#6676,
#6677,#6678,#6679,#6680,#6681),(#6682,#6683,#6684,#6685,#6686,#6687,#6688,
#6689,#6690,#6691,#6692,#6693,#6694,#6695,#6696,#6697,#6698,#6699,#6700,
#6701,#6702,#6703,#6704,#6705,#6706,#6707,#6708,#6709,#6710,#6711,#6712,
#6713,#6714,#6715,#6716,#6717,#6718,#6719,#6720,#6721,#6722,#6723,#6724,
#6725,#6726,#6727,#6728,#6729,#6730,#6731,#6732,#6733,#6734,#6735,#6736,
#6737,#6738,#6739,#6740,#6741,#6742)),.UNSPECIFIED.,.T.,.F.,.F.,(4,1,1,
1,1,1,1,1,4),(4,1,1,1,1,1,1,1,1,1,1,1,1,1,1,1,1,1,1,1,1,1,1,1,1,1,1,1,1,
1,1,1,1,1,1,1,1,1,1,1,1,1,1,1,1,1,1,1,1,1,1,1,1,1,1,1,1,1,4),(-3.14159265358979,
-2.46839422782055,-2.24399475256414,-1.34639685153848,-0.448798950512828,
0.448798950512828,1.34639685153848,2.24399475256414,3.14159265358979),(0.,
0.0178571428571429,0.0357142857142857,0.0535714285714286,0.0714285714285714,
0.0892857142857143,0.107142857142857,0.125,0.129464285714286,0.133928571428571,
0.138392857142857,0.142857142857143,0.166666666666667,0.19047619047619,
0.214285714285714,0.232142857142857,0.25,0.267857142857143,0.285714285714286,
0.303571428571429,0.321428571428571,0.339285714285714,0.357142857142857,
0.375,0.392857142857143,0.410714285714286,0.428571428571429,0.446428571428571,
0.464285714285714,0.482142857142857,0.5,0.517857142857143,0.535714285714286,
0.553571428571429,0.571428571428571,0.589285714285714,0.607142857142857,
0.625,0.642857142857143,0.666666666666667,0.69047619047619,0.714285714285714,
0.726190476190476,0.738095238095238,0.761904761904762,0.767857142857143,
0.773809523809524,0.785714285714286,0.809523809523809,0.833333333333333,
0.857142857142857,0.875,0.892857142857143,0.910714285714286,0.928571428571429,
0.946428571428571,0.964285714285714,0.982142857142857,1.),.UNSPECIFIED.);
#166=B_SPLINE_SURFACE_WITH_KNOTS('',3,3,((#7043,#7044,#7045,#7046,#7047,
#7048,#7049,#7050,#7051,#7052,#7053,#7054,#7055,#7056,#7057,#7058,#7059,
#7060,#7061,#7062,#7063,#7064,#7065,#7066,#7067,#7068,#7069,#7070,#7071,
#7072,#7073,#7074,#7075,#7076,#7077,#7078,#7079,#7080,#7081,#7082,#7083,
#7084,#7085,#7086,#7087,#7088,#7089,#7090,#7091,#7092,#7093,#7094,#7095,
#7096,#7097,#7098,#7099,#7100,#7101,#7102,#7103,#7104,#7105,#7106,#7107,
#7108,#7109,#7110,#7111,#7112,#7113),(#7114,#7115,#7116,#7117,#7118,#7119,
#7120,#7121,#7122,#7123,#7124,#7125,#7126,#7127,#7128,#7129,#7130,#7131,
#7132,#7133,#7134,#7135,#7136,#7137,#7138,#7139,#7140,#7141,#7142,#7143,
#7144,#7145,#7146,#7147,#7148,#7149,#7150,#7151,#7152,#7153,#7154,#7155,
#7156,#7157,#7158,#7159,#7160,#7161,#7162,#7163,#7164,#7165,#7166,#7167,
#7168,#7169,#7170,#7171,#7172,#7173,#7174,#7175,#7176,#7177,#7178,#7179,
#7180,#7181,#7182,#7183,#7184),(#7185,#7186,#7187,#7188,#7189,#7190,#7191,
#7192,#7193,#7194,#7195,#7196,#7197,#7198,#7199,#7200,#7201,#7202,#7203,
#7204,#7205,#7206,#7207,#7208,#7209,#7210,#7211,#7212,#7213,#7214,#7215,
#7216,#7217,#7218,#7219,#7220,#7221,#7222,#7223,#7224,#7225,#7226,#7227,
#7228,#7229,#7230,#7231,#7232,#7233,#7234,#7235,#7236,#7237,#7238,#7239,
#7240,#7241,#7242,#7243,#7244,#7245,#7246,#7247,#7248,#7249,#7250,#7251,
#7252,#7253,#7254,#7255),(#7256,#7257,#7258,#7259,#7260,#7261,#7262,#7263,
#7264,#7265,#7266,#7267,#7268,#7269,#7270,#7271,#7272,#7273,#7274,#7275,
#7276,#7277,#7278,#7279,#7280,#7281,#7282,#7283,#7284,#7285,#7286,#7287,
#7288,#7289,#7290,#7291,#7292,#7293,#7294,#7295,#7296,#7297,#7298,#7299,
#7300,#7301,#7302,#7303,#7304,#7305,#7306,#7307,#7308,#7309,#7310,#7311,
#7312,#7313,#7314,#7315,#7316,#7317,#7318,#7319,#7320,#7321,#7322,#7323,
#7324,#7325,#7326),(#7327,#7328,#7329,#7330,#7331,#7332,#7333,#7334,#7335,
#7336,#7337,#7338,#7339,#7340,#7341,#7342,#7343,#7344,#7345,#7346,#7347,
#7348,#7349,#7350,#7351,#7352,#7353,#7354,#7355,#7356,#7357,#7358,#7359,
#7360,#7361,#7362,#7363,#7364,#7365,#7366,#7367,#7368,#7369,#7370,#7371,
#7372,#7373,#7374,#7375,#7376,#7377,#7378,#7379,#7380,#7381,#7382,#7383,
#7384,#7385,#7386,#7387,#7388,#7389,#7390,#7391,#7392,#7393,#7394,#7395,
#7396,#7397),(#7398,#7399,#7400,#7401,#7402,#7403,#7404,#7405,#7406,#7407,
#7408,#7409,#7410,#7411,#7412,#7413,#7414,#7415,#7416,#7417,#7418,#7419,
#7420,#7421,#7422,#7423,#7424,#7425,#7426,#7427,#7428,#7429,#7430,#7431,
#7432,#7433,#7434,#7435,#7436,#7437,#7438,#7439,#7440,#7441,#7442,#7443,
#7444,#7445,#7446,#7447,#7448,#7449,#7450,#7451,#7452,#7453,#7454,#7455,
#7456,#7457,#7458,#7459,#7460,#7461,#7462,#7463,#7464,#7465,#7466,#7467,
#7468),(#7469,#7470,#7471,#7472,#7473,#7474,#7475,#7476,#7477,#7478,#7479,
#7480,#7481,#7482,#7483,#7484,#7485,#7486,#7487,#7488,#7489,#7490,#7491,
#7492,#7493,#7494,#7495,#7496,#7497,#7498,#7499,#7500,#7501,#7502,#7503,
#7504,#7505,#7506,#7507,#7508,#7509,#7510,#7511,#7512,#7513,#7514,#7515,
#7516,#7517,#7518,#7519,#7520,#7521,#7522,#7523,#7524,#7525,#7526,#7527,
#7528,#7529,#7530,#7531,#7532,#7533,#7534,#7535,#7536,#7537,#7538,#7539),
(#7540,#7541,#7542,#7543,#7544,#7545,#7546,#7547,#7548,#7549,#7550,#7551,
#7552,#7553,#7554,#7555,#7556,#7557,#7558,#7559,#7560,#7561,#7562,#7563,
#7564,#7565,#7566,#7567,#7568,#7569,#7570,#7571,#7572,#7573,#7574,#7575,
#7576,#7577,#7578,#7579,#7580,#7581,#7582,#7583,#7584,#7585,#7586,#7587,
#7588,#7589,#7590,#7591,#7592,#7593,#7594,#7595,#7596,#7597,#7598,#7599,
#7600,#7601,#7602,#7603,#7604,#7605,#7606,#7607,#7608,#7609,#7610),(#7611,
#7612,#7613,#7614,#7615,#7616,#7617,#7618,#7619,#7620,#7621,#7622,#7623,
#7624,#7625,#7626,#7627,#7628,#7629,#7630,#7631,#7632,#7633,#7634,#7635,
#7636,#7637,#7638,#7639,#7640,#7641,#7642,#7643,#7644,#7645,#7646,#7647,
#7648,#7649,#7650,#7651,#7652,#7653,#7654,#7655,#7656,#7657,#7658,#7659,
#7660,#7661,#7662,#7663,#7664,#7665,#7666,#7667,#7668,#7669,#7670,#7671,
#7672,#7673,#7674,#7675,#7676,#7677,#7678,#7679,#7680,#7681),(#7682,#7683,
#7684,#7685,#7686,#7687,#7688,#7689,#7690,#7691,#7692,#7693,#7694,#7695,
#7696,#7697,#7698,#7699,#7700,#7701,#7702,#7703,#7704,#7705,#7706,#7707,
#7708,#7709,#7710,#7711,#7712,#7713,#7714,#7715,#7716,#7717,#7718,#7719,
#7720,#7721,#7722,#7723,#7724,#7725,#7726,#7727,#7728,#7729,#7730,#7731,
#7732,#7733,#7734,#7735,#7736,#7737,#7738,#7739,#7740,#7741,#7742,#7743,
#7744,#7745,#7746,#7747,#7748,#7749,#7750,#7751,#7752)),.UNSPECIFIED.,.T.,
 .F.,.F.,(4,1,1,1,1,1,1,4),(4,1,1,1,1,1,1,1,1,1,1,1,1,1,1,1,1,1,1,1,1,1,
1,1,1,1,1,1,1,1,1,1,1,1,1,1,1,1,1,1,1,1,1,1,1,1,1,1,1,1,1,1,1,1,1,1,1,1,
1,1,1,1,1,1,1,1,1,1,4),(-3.14159265358979,-2.24399475256414,-1.34639685153848,
-0.448798950512828,0.448798950512828,1.34639685153848,2.24399475256414,
3.14159265358979),(0.,0.0178571428571429,0.0357142857142857,0.0535714285714286,
0.0714285714285714,0.0892857142857143,0.107142857142857,0.125,0.142857142857143,
0.150793650793651,0.158730158730159,0.174603174603175,0.19047619047619,
0.202380952380952,0.214285714285714,0.226190476190476,0.238095238095238,
0.25,0.261904761904762,0.267857142857143,0.273809523809524,0.285714285714286,
0.297619047619048,0.30952380952381,0.321428571428571,0.333333333333333,
0.349206349206349,0.365079365079365,0.380952380952381,0.396825396825397,
0.412698412698413,0.428571428571429,0.446428571428571,0.464285714285714,
0.476190476190476,0.488095238095238,0.5,0.517857142857143,0.535714285714286,
0.553571428571429,0.571428571428571,0.589285714285714,0.607142857142857,
0.625,0.642857142857143,0.660714285714286,0.678571428571428,0.696428571428571,
0.714285714285714,0.726190476190476,0.738095238095238,0.75,0.761904761904762,
0.773809523809524,0.785714285714286,0.797619047619047,0.809523809523809,
0.821428571428571,0.833333333333333,0.845238095238095,0.857142857142857,
0.875,0.892857142857143,0.910714285714286,0.928571428571429,0.946428571428571,
0.964285714285714,0.982142857142857,1.),.UNSPECIFIED.);
#167=B_SPLINE_CURVE_WITH_KNOTS('',3,(#5773,#5774,#5775,#5776,#5777,#5778,
#5779,#5780,#5781,#5782,#5783,#5784,#5785,#5786,#5787,#5788,#5789,#5790),
 .UNSPECIFIED.,.F.,.F.,(4,2,2,2,2,2,2,2,4),(0.603815071984235,0.754767131302978,
0.90571919062172,1.0566746672951,1.20763014396847,1.35858562064185,1.50954109731522,
1.66049315663396,1.81144521595271),.UNSPECIFIED.);
#168=B_SPLINE_CURVE_WITH_KNOTS('',3,(#5793,#5794,#5795,#5796,#5797,#5798,
#5799,#5800,#5801,#5802,#5803,#5804,#5805,#5806,#5807,#5808,#5809,#5810,
#5811),.UNSPECIFIED.,.F.,.F.,(4,2,2,2,3,2,2,2,4),(1.81144521595271,1.96239727527145,
2.11334933459019,2.26430481126357,2.41526028793694,2.56621576461032,2.71717124128369,
2.86812330060244,3.01907535992118),.UNSPECIFIED.);
#169=B_SPLINE_CURVE_WITH_KNOTS('',3,(#5826,#5827,#5828,#5829,#5830,#5831,
#5832,#5833,#5834,#5835,#5836,#5837,#5838,#5839,#5840,#5841,#5842,#5843,
#5844,#5845,#5846,#5847,#5848,#5849,#5850,#5851),.UNSPECIFIED.,.F.,.F.,
(4,2,2,2,2,2,2,2,2,2,2,2,4),(0.,0.258582759599652,0.517165519199304,0.775740569348226,
1.03431561949715,1.29289066964607,1.55146571979499,1.81004847939464,2.0686312389943,
2.32721399859395,2.5857967581936,2.84437180834252,3.10294685849144),
 .UNSPECIFIED.);
#170=B_SPLINE_CURVE_WITH_KNOTS('',3,(#5852,#5853,#5854,#5855,#5856,#5857,
#5858,#5859,#5860,#5861),.UNSPECIFIED.,.F.,.F.,(4,2,2,2,4),(3.10294685849144,
3.36152190864037,3.62009695878929,3.87867971838894,4.13726247798859),
 .UNSPECIFIED.);
#171=B_SPLINE_CURVE_WITH_KNOTS('',3,(#5868,#5869,#5870,#5871,#5872,#5873,
#5874,#5875,#5876,#5877,#5878,#5879,#5880,#5881,#5882,#5883,#5884,#5885),
 .UNSPECIFIED.,.F.,.F.,(4,2,2,2,2,2,2,2,4),(0.615024883366032,0.768571244696458,
0.922117606026885,1.07608368637947,1.23004976673206,1.38401584708465,1.53798192743724,
1.69152828876767,1.8450746500981),.UNSPECIFIED.);
#172=B_SPLINE_CURVE_WITH_KNOTS('',3,(#5889,#5890,#5891,#5892,#5893,#5894,
#5895,#5896,#5897,#5898,#5899,#5900,#5901,#5902,#5903,#5904,#5905,#5906,
#5907),.UNSPECIFIED.,.F.,.F.,(4,2,2,2,3,2,2,2,4),(1.8450746500981,1.99862101142852,
2.15216737275895,2.30613345311154,2.46009953346413,2.61406561381672,2.76803169416931,
2.92157805549973,3.07512441683016),.UNSPECIFIED.);
#173=B_SPLINE_CURVE_WITH_KNOTS('',3,(#5916,#5917,#5918,#5919,#5920,#5921,
#5922,#5923,#5924,#5925),.UNSPECIFIED.,.F.,.F.,(4,2,2,2,4),(0.,0.258582759599652,
0.517165519199304,0.775740569348226,1.03431561949715),.UNSPECIFIED.);
#174=B_SPLINE_CURVE_WITH_KNOTS('',3,(#5927,#5928,#5929,#5930,#5931,#5932,
#5933,#5934,#5935,#5936),.UNSPECIFIED.,.F.,.F.,(4,2,2,2,4),(3.10294685849144,
3.36152190864037,3.62009695878929,3.87867971838894,4.13726247798859),
 .UNSPECIFIED.);
#175=B_SPLINE_CURVE_WITH_KNOTS('',3,(#5937,#5938,#5939,#5940,#5941,#5942,
#5943,#5944,#5945,#5946,#5947,#5948,#5949,#5950,#5951,#5952,#5953,#5954),
 .UNSPECIFIED.,.F.,.F.,(4,2,2,2,2,2,2,2,4),(1.03431561949715,1.29289066964607,
1.55146571979499,1.81004847939464,2.0686312389943,2.32721399859395,2.5857967581936,
2.84437180834252,3.10294685849144),.UNSPECIFIED.);
#176=B_SPLINE_CURVE_WITH_KNOTS('',3,(#6746,#6747,#6748,#6749,#6750,#6751,
#6752,#6753,#6754,#6755,#6756,#6757,#6758,#6759,#6760,#6761,#6762,#6763,
#6764,#6765,#6766,#6767,#6768,#6769,#6770,#6771,#6772,#6773,#6774,#6775,
#6776,#6777,#6778,#6779,#6780,#6781,#6782,#6783,#6784,#6785,#6786,#6787,
#6788,#6789,#6790,#6791,#6792,#6793,#6794,#6795,#6796,#6797,#6798,#6799,
#6800,#6801,#6802,#6803,#6804,#6805,#6806),.UNSPECIFIED.,.F.,.F.,(4,1,1,
1,1,1,1,1,1,1,1,1,1,1,1,1,1,1,1,1,1,1,1,1,1,1,1,1,1,1,1,1,1,1,1,1,1,1,1,
1,1,1,1,1,1,1,1,1,1,1,1,1,1,1,1,1,1,1,4),(0.,0.0178571428571429,0.0357142857142857,
0.0535714285714286,0.0714285714285714,0.0892857142857143,0.107142857142857,
0.125,0.129464285714286,0.133928571428571,0.138392857142857,0.142857142857143,
0.166666666666667,0.19047619047619,0.214285714285714,0.232142857142857,
0.25,0.267857142857143,0.285714285714286,0.303571428571429,0.321428571428571,
0.339285714285714,0.357142857142857,0.375,0.392857142857143,0.410714285714286,
0.428571428571429,0.446428571428571,0.464285714285714,0.482142857142857,
0.5,0.517857142857143,0.535714285714286,0.553571428571429,0.571428571428571,
0.589285714285714,0.607142857142857,0.625,0.642857142857143,0.666666666666667,
0.69047619047619,0.714285714285714,0.726190476190476,0.738095238095238,
0.761904761904762,0.767857142857143,0.773809523809524,0.785714285714286,
0.809523809523809,0.833333333333333,0.857142857142857,0.875,0.892857142857143,
0.910714285714286,0.928571428571429,0.946428571428571,0.964285714285714,
0.982142857142857,1.),.UNSPECIFIED.);
#177=B_SPLINE_CURVE_WITH_KNOTS('',3,(#7756,#7757,#7758,#7759,#7760,#7761,
#7762,#7763,#7764,#7765,#7766,#7767,#7768,#7769,#7770,#7771,#7772,#7773,
#7774,#7775,#7776,#7777,#7778,#7779,#7780,#7781,#7782,#7783,#7784,#7785,
#7786,#7787,#7788,#7789,#7790,#7791,#7792,#7793,#7794,#7795,#7796,#7797,
#7798,#7799,#7800,#7801,#7802,#7803,#7804,#7805,#7806,#7807,#7808,#7809,
#7810,#7811,#7812,#7813,#7814,#7815,#7816,#7817,#7818,#7819,#7820,#7821,
#7822,#7823,#7824,#7825,#7826),.UNSPECIFIED.,.F.,.F.,(4,1,1,1,1,1,1,1,1,
1,1,1,1,1,1,1,1,1,1,1,1,1,1,1,1,1,1,1,1,1,1,1,1,1,1,1,1,1,1,1,1,1,1,1,1,
1,1,1,1,1,1,1,1,1,1,1,1,1,1,1,1,1,1,1,1,1,1,1,4),(0.,0.0178571428571429,
0.0357142857142857,0.0535714285714286,0.0714285714285714,0.0892857142857143,
0.107142857142857,0.125,0.142857142857143,0.150793650793651,0.158730158730159,
0.174603174603175,0.19047619047619,0.202380952380952,0.214285714285714,
0.226190476190476,0.238095238095238,0.25,0.261904761904762,0.267857142857143,
0.273809523809524,0.285714285714286,0.297619047619048,0.30952380952381,
0.321428571428571,0.333333333333333,0.349206349206349,0.365079365079365,
0.380952380952381,0.396825396825397,0.412698412698413,0.428571428571429,
0.446428571428571,0.464285714285714,0.476190476190476,0.488095238095238,
0.5,0.517857142857143,0.535714285714286,0.553571428571429,0.571428571428571,
0.589285714285714,0.607142857142857,0.625,0.642857142857143,0.660714285714286,
0.678571428571428,0.696428571428571,0.714285714285714,0.726190476190476,
0.738095238095238,0.75,0.761904761904762,0.773809523809524,0.785714285714286,
0.797619047619047,0.809523809523809,0.821428571428571,0.833333333333333,
0.845238095238095,0.857142857142857,0.875,0.892857142857143,0.910714285714286,
0.928571428571429,0.946428571428571,0.964285714285714,0.982142857142857,
1.),.UNSPECIFIED.);
#178=B_SPLINE_CURVE_WITH_KNOTS('',3,(#7865,#7866,#7867,#7868,#7869,#7870,
#7871,#7872,#7873,#7874),.UNSPECIFIED.,.F.,.F.,(4,2,2,2,4),(0.665271585430993,
0.692803751398642,0.755746158887619,0.818688566376595,0.846220732344244),
 .UNSPECIFIED.);
#179=B_SPLINE_CURVE_WITH_KNOTS('',3,(#7877,#7878,#7879,#7880,#7881,#7882,
#7883,#7884,#7885,#7886),.UNSPECIFIED.,.F.,.F.,(4,2,2,2,4),(0.161440812839248,
0.188972978806896,0.251915386295873,0.314857793784849,0.342389959752498),
 .UNSPECIFIED.);
#180=B_SPLINE_CURVE_WITH_KNOTS('',3,(#7889,#7890,#7891,#7892,#7893,#7894,
#7895,#7896,#7897,#7898,#7899,#7900,#7901,#7902,#7903,#7904,#7905,#7906,
#7907,#7908,#7909,#7910,#7911,#7912,#7913,#7914,#7915,#7916,#7917,#7918,
#7919,#7920,#7921,#7922),.UNSPECIFIED.,.T.,.F.,(4,2,2,2,2,2,2,2,2,2,2,2,
2,2,2,2,4),(0.,0.0622075173149514,0.124415034629903,0.186622241324509,0.248829448019115,
0.311036654713721,0.373243861408326,0.435451378723278,0.497658896038229,
0.559866413353181,0.622073930668132,0.684281137362738,0.746488344057344,
0.80869555075195,0.870902757446556,0.933110274761507,0.995317792076459),
 .UNSPECIFIED.);
#181=SHAPE_REPRESENTATION_RELATIONSHIP('SRR','None',#8515,#205);
#182=SHAPE_REPRESENTATION_RELATIONSHIP('SRR','None',#8516,#206);
#183=SHAPE_REPRESENTATION_RELATIONSHIP('SRR','None',#8517,#207);
#184=SHAPE_REPRESENTATION_RELATIONSHIP('SRR','None',#8518,#208);
#185=SHAPE_REPRESENTATION_RELATIONSHIP('SRR','None',#8519,#209);
#186=SHAPE_REPRESENTATION_RELATIONSHIP('SRR','None',#8520,#210);
#187=SHAPE_REPRESENTATION_RELATIONSHIP('SRR','None',#8521,#211);
#188=SHAPE_REPRESENTATION_RELATIONSHIP('SRR','None',#8522,#212);
#189=SHAPE_REPRESENTATION_RELATIONSHIP('SRR','None',#8523,#213);
#190=SHAPE_REPRESENTATION_RELATIONSHIP('SRR','None',#8524,#214);
#191=SHAPE_REPRESENTATION_RELATIONSHIP('SRR','None',#8525,#215);
#192=SHAPE_REPRESENTATION_RELATIONSHIP('SRR','None',#8526,#216);
#193=SHAPE_REPRESENTATION_RELATIONSHIP('SRR','None',#8527,#217);
#194=SHAPE_REPRESENTATION_RELATIONSHIP('SRR','None',#8528,#218);
#195=SHAPE_REPRESENTATION_RELATIONSHIP('SRR','None',#8529,#219);
#196=SHAPE_REPRESENTATION_RELATIONSHIP('SRR','None',#8530,#220);
#197=SHAPE_REPRESENTATION_RELATIONSHIP('SRR','None',#8531,#221);
#198=SHAPE_REPRESENTATION_RELATIONSHIP('SRR','None',#8532,#222);
#199=SHAPE_REPRESENTATION_RELATIONSHIP('SRR','None',#8533,#223);
#200=SHAPE_REPRESENTATION_RELATIONSHIP('SRR','None',#8534,#224);
#201=SHAPE_REPRESENTATION_RELATIONSHIP('SRR','None',#8535,#225);
#202=SHAPE_REPRESENTATION_RELATIONSHIP('SRR','None',#8536,#226);
#203=SHAPE_REPRESENTATION_RELATIONSHIP('SRR','None',#8537,#227);
#204=SHAPE_REPRESENTATION_RELATIONSHIP('SRR','None',#8538,#228);
#205=ADVANCED_BREP_SHAPE_REPRESENTATION('',(#253),#8404);
#206=ADVANCED_BREP_SHAPE_REPRESENTATION('',(#254),#8405);
#207=ADVANCED_BREP_SHAPE_REPRESENTATION('',(#255),#8406);
#208=ADVANCED_BREP_SHAPE_REPRESENTATION('',(#256),#8407);
#209=ADVANCED_BREP_SHAPE_REPRESENTATION('',(#257),#8408);
#210=ADVANCED_BREP_SHAPE_REPRESENTATION('',(#258),#8409);
#211=ADVANCED_BREP_SHAPE_REPRESENTATION('',(#259),#8410);
#212=ADVANCED_BREP_SHAPE_REPRESENTATION('',(#260),#8411);
#213=ADVANCED_BREP_SHAPE_REPRESENTATION('',(#261),#8412);
#214=ADVANCED_BREP_SHAPE_REPRESENTATION('',(#262),#8413);
#215=ADVANCED_BREP_SHAPE_REPRESENTATION('',(#263),#8414);
#216=ADVANCED_BREP_SHAPE_REPRESENTATION('',(#264),#8415);
#217=ADVANCED_BREP_SHAPE_REPRESENTATION('',(#265),#8416);
#218=ADVANCED_BREP_SHAPE_REPRESENTATION('',(#266),#8417);
#219=ADVANCED_BREP_SHAPE_REPRESENTATION('',(#267),#8418);
#220=ADVANCED_BREP_SHAPE_REPRESENTATION('',(#268),#8419);
#221=ADVANCED_BREP_SHAPE_REPRESENTATION('',(#269),#8420);
#222=ADVANCED_BREP_SHAPE_REPRESENTATION('',(#270),#8421);
#223=ADVANCED_BREP_SHAPE_REPRESENTATION('',(#163),#8422);
#224=ADVANCED_BREP_SHAPE_REPRESENTATION('',(#271),#8423);
#225=ADVANCED_BREP_SHAPE_REPRESENTATION('',(#164),#8424);
#226=ADVANCED_BREP_SHAPE_REPRESENTATION('',(#272),#8425);
#227=ADVANCED_BREP_SHAPE_REPRESENTATION('',(#273),#8426);
#228=ADVANCED_BREP_SHAPE_REPRESENTATION('',(#274),#8427);
#229=STYLED_ITEM('',(#8684),#253);
#230=STYLED_ITEM('',(#8698),#254);
#231=STYLED_ITEM('',(#8698),#255);
#232=STYLED_ITEM('',(#8684),#256);
#233=STYLED_ITEM('',(#8698),#257);
#234=STYLED_ITEM('',(#8719),#258);
#235=STYLED_ITEM('',(#8719),#259);
#236=STYLED_ITEM('',(#8705),#260);
#237=STYLED_ITEM('',(#8719),#261);
#238=STYLED_ITEM('',(#8719),#262);
#239=STYLED_ITEM('',(#8698),#263);
#240=STYLED_ITEM('',(#8698),#264);
#241=STYLED_ITEM('',(#8705),#265);
#242=STYLED_ITEM('',(#8705),#266);
#243=STYLED_ITEM('',(#8712),#267);
#244=STYLED_ITEM('',(#8691),#268);
#245=STYLED_ITEM('',(#8698),#269);
#246=STYLED_ITEM('',(#8698),#270);
#247=STYLED_ITEM('',(#8712),#163);
#248=STYLED_ITEM('',(#8698),#271);
#249=STYLED_ITEM('',(#8712),#164);
#250=STYLED_ITEM('',(#8712),#272);
#251=STYLED_ITEM('',(#8712),#273);
#252=STYLED_ITEM('',(#8712),#274);
#253=MANIFOLD_SOLID_BREP('Body1',#3675);
#254=MANIFOLD_SOLID_BREP('Body1',#3676);
#255=MANIFOLD_SOLID_BREP('Body1',#3677);
#256=MANIFOLD_SOLID_BREP('Body1',#3678);
#257=MANIFOLD_SOLID_BREP('Body1',#3679);
#258=MANIFOLD_SOLID_BREP('Body1',#3680);
#259=MANIFOLD_SOLID_BREP('Body1',#3681);
#260=MANIFOLD_SOLID_BREP('Body1',#3682);
#261=MANIFOLD_SOLID_BREP('Body1',#3683);
#262=MANIFOLD_SOLID_BREP('Body1',#3684);
#263=MANIFOLD_SOLID_BREP('Body1',#3685);
#264=MANIFOLD_SOLID_BREP('Body1',#3686);
#265=MANIFOLD_SOLID_BREP('Body1',#3687);
#266=MANIFOLD_SOLID_BREP('Body1',#3688);
#267=MANIFOLD_SOLID_BREP('Body1',#3689);
#268=MANIFOLD_SOLID_BREP('Body1',#3690);
#269=MANIFOLD_SOLID_BREP('Body1',#3691);
#270=MANIFOLD_SOLID_BREP('Body1',#3692);
#271=MANIFOLD_SOLID_BREP('Body1',#3695);
#272=MANIFOLD_SOLID_BREP('Body1',#3698);
#273=MANIFOLD_SOLID_BREP('Body1',#3699);
#274=MANIFOLD_SOLID_BREP('Body1',#3700);
#275=FACE_BOUND('',#735,.T.);
#276=FACE_BOUND('',#736,.T.);
#277=FACE_BOUND('',#738,.T.);
#278=FACE_BOUND('',#739,.T.);
#279=FACE_BOUND('',#746,.T.);
#280=FACE_BOUND('',#748,.T.);
#281=FACE_BOUND('',#755,.T.);
#282=FACE_BOUND('',#757,.T.);
#283=FACE_BOUND('',#779,.T.);
#284=FACE_BOUND('',#788,.T.);
#285=FACE_BOUND('',#791,.T.);
#286=FACE_BOUND('',#793,.T.);
#287=FACE_BOUND('',#795,.T.);
#288=FACE_BOUND('',#796,.T.);
#289=FACE_BOUND('',#797,.T.);
#290=FACE_BOUND('',#798,.T.);
#291=FACE_BOUND('',#799,.T.);
#292=FACE_BOUND('',#800,.T.);
#293=FACE_BOUND('',#801,.T.);
#294=FACE_BOUND('',#803,.T.);
#295=FACE_BOUND('',#804,.T.);
#296=FACE_BOUND('',#805,.T.);
#297=FACE_BOUND('',#807,.T.);
#298=FACE_BOUND('',#815,.T.);
#299=FACE_BOUND('',#817,.T.);
#300=FACE_BOUND('',#819,.T.);
#301=FACE_BOUND('',#822,.T.);
#302=FACE_BOUND('',#824,.T.);
#303=FACE_BOUND('',#831,.T.);
#304=FACE_BOUND('',#839,.T.);
#305=FACE_BOUND('',#841,.T.);
#306=FACE_BOUND('',#851,.T.);
#307=FACE_BOUND('',#852,.T.);
#308=FACE_BOUND('',#853,.T.);
#309=FACE_BOUND('',#854,.T.);
#310=FACE_BOUND('',#855,.T.);
#311=FACE_BOUND('',#856,.T.);
#312=FACE_BOUND('',#857,.T.);
#313=FACE_BOUND('',#859,.T.);
#314=FACE_BOUND('',#860,.T.);
#315=FACE_BOUND('',#861,.T.);
#316=FACE_BOUND('',#862,.T.);
#317=FACE_BOUND('',#863,.T.);
#318=FACE_BOUND('',#864,.T.);
#319=FACE_BOUND('',#865,.T.);
#320=FACE_BOUND('',#869,.T.);
#321=FACE_BOUND('',#871,.T.);
#322=FACE_BOUND('',#875,.T.);
#323=FACE_BOUND('',#877,.T.);
#324=FACE_BOUND('',#900,.T.);
#325=FACE_BOUND('',#902,.T.);
#326=FACE_BOUND('',#905,.T.);
#327=FACE_BOUND('',#906,.T.);
#328=FACE_BOUND('',#907,.T.);
#329=FACE_BOUND('',#908,.T.);
#330=FACE_BOUND('',#909,.T.);
#331=FACE_BOUND('',#910,.T.);
#332=FACE_BOUND('',#911,.T.);
#333=FACE_BOUND('',#913,.T.);
#334=FACE_BOUND('',#914,.T.);
#335=FACE_BOUND('',#915,.T.);
#336=FACE_BOUND('',#916,.T.);
#337=FACE_BOUND('',#917,.T.);
#338=FACE_BOUND('',#918,.T.);
#339=FACE_BOUND('',#919,.T.);
#340=FACE_BOUND('',#928,.T.);
#341=FACE_BOUND('',#936,.T.);
#342=FACE_BOUND('',#938,.T.);
#343=FACE_BOUND('',#940,.T.);
#344=FACE_BOUND('',#942,.T.);
#345=FACE_BOUND('',#960,.T.);
#346=FACE_BOUND('',#974,.T.);
#347=FACE_BOUND('',#976,.T.);
#348=FACE_BOUND('',#985,.T.);
#349=FACE_BOUND('',#990,.T.);
#350=FACE_BOUND('',#997,.T.);
#351=FACE_BOUND('',#1013,.T.);
#352=FACE_BOUND('',#1015,.T.);
#353=FACE_BOUND('',#1026,.T.);
#354=FACE_BOUND('',#1028,.T.);
#355=FACE_BOUND('',#1037,.T.);
#356=PLANE('',#3974);
#357=PLANE('',#3975);
#358=PLANE('',#3976);
#359=PLANE('',#3977);
#360=PLANE('',#3978);
#361=PLANE('',#3979);
#362=PLANE('',#3984);
#363=PLANE('',#3985);
#364=PLANE('',#3986);
#365=PLANE('',#3987);
#366=PLANE('',#3988);
#367=PLANE('',#3989);
#368=PLANE('',#3994);
#369=PLANE('',#3995);
#370=PLANE('',#3996);
#371=PLANE('',#3997);
#372=PLANE('',#3998);
#373=PLANE('',#3999);
#374=PLANE('',#4004);
#375=PLANE('',#4008);
#376=PLANE('',#4012);
#377=PLANE('',#4016);
#378=PLANE('',#4020);
#379=PLANE('',#4024);
#380=PLANE('',#4029);
#381=PLANE('',#4031);
#382=PLANE('',#4041);
#383=PLANE('',#4045);
#384=PLANE('',#4049);
#385=PLANE('',#4053);
#386=PLANE('',#4057);
#387=PLANE('',#4061);
#388=PLANE('',#4065);
#389=PLANE('',#4066);
#390=PLANE('',#4068);
#391=PLANE('',#4073);
#392=PLANE('',#4076);
#393=PLANE('',#4084);
#394=PLANE('',#4085);
#395=PLANE('',#4087);
#396=PLANE('',#4092);
#397=PLANE('',#4095);
#398=PLANE('',#4102);
#399=PLANE('',#4106);
#400=PLANE('',#4107);
#401=PLANE('',#4111);
#402=PLANE('',#4112);
#403=PLANE('',#4120);
#404=PLANE('',#4121);
#405=PLANE('',#4147);
#406=PLANE('',#4148);
#407=PLANE('',#4156);
#408=PLANE('',#4157);
#409=PLANE('',#4164);
#410=PLANE('',#4165);
#411=PLANE('',#4167);
#412=PLANE('',#4175);
#413=PLANE('',#4177);
#414=PLANE('',#4182);
#415=PLANE('',#4187);
#416=PLANE('',#4195);
#417=PLANE('',#4230);
#418=PLANE('',#4231);
#419=PLANE('',#4235);
#420=PLANE('',#4236);
#421=PLANE('',#4240);
#422=PLANE('',#4241);
#423=PLANE('',#4246);
#424=PLANE('',#4250);
#425=PLANE('',#4251);
#426=PLANE('',#4256);
#427=PLANE('',#4257);
#428=PLANE('',#4259);
#429=PLANE('',#4264);
#430=PLANE('',#4271);
#431=PLANE('',#4272);
#432=PLANE('',#4274);
#433=PLANE('',#4275);
#434=PLANE('',#4276);
#435=PLANE('',#4277);
#436=PLANE('',#4278);
#437=PLANE('',#4279);
#438=PLANE('',#4281);
#439=PLANE('',#4282);
#440=PLANE('',#4283);
#441=PLANE('',#4284);
#442=PLANE('',#4285);
#443=PLANE('',#4286);
#444=PLANE('',#4288);
#445=PLANE('',#4296);
#446=PLANE('',#4304);
#447=PLANE('',#4305);
#448=PLANE('',#4306);
#449=PLANE('',#4307);
#450=PLANE('',#4308);
#451=PLANE('',#4309);
#452=PLANE('',#4310);
#453=PLANE('',#4311);
#454=PLANE('',#4312);
#455=PLANE('',#4314);
#456=PLANE('',#4316);
#457=PLANE('',#4318);
#458=PLANE('',#4319);
#459=PLANE('',#4320);
#460=PLANE('',#4321);
#461=PLANE('',#4322);
#462=PLANE('',#4323);
#463=PLANE('',#4326);
#464=PLANE('',#4334);
#465=PLANE('',#4338);
#466=PLANE('',#4346);
#467=PLANE('',#4354);
#468=PLANE('',#4355);
#469=PLANE('',#4356);
#470=PLANE('',#4357);
#471=PLANE('',#4358);
#472=PLANE('',#4359);
#473=PLANE('',#4360);
#474=PLANE('',#4361);
#475=PLANE('',#4362);
#476=PLANE('',#4370);
#477=PLANE('',#4371);
#478=PLANE('',#4377);
#479=PLANE('',#4378);
#480=PLANE('',#4379);
#481=PLANE('',#4383);
#482=PLANE('',#4384);
#483=PLANE('',#4385);
#484=PLANE('',#4386);
#485=PLANE('',#4387);
#486=PLANE('',#4389);
#487=PLANE('',#4390);
#488=PLANE('',#4391);
#489=PLANE('',#4392);
#490=PLANE('',#4393);
#491=PLANE('',#4394);
#492=PLANE('',#4395);
#493=PLANE('',#4396);
#494=PLANE('',#4404);
#495=FACE_OUTER_BOUND('',#728,.T.);
#496=FACE_OUTER_BOUND('',#729,.T.);
#497=FACE_OUTER_BOUND('',#730,.T.);
#498=FACE_OUTER_BOUND('',#731,.T.);
#499=FACE_OUTER_BOUND('',#732,.T.);
#500=FACE_OUTER_BOUND('',#733,.T.);
#501=FACE_OUTER_BOUND('',#734,.T.);
#502=FACE_OUTER_BOUND('',#737,.T.);
#503=FACE_OUTER_BOUND('',#740,.T.);
#504=FACE_OUTER_BOUND('',#741,.T.);
#505=FACE_OUTER_BOUND('',#742,.T.);
#506=FACE_OUTER_BOUND('',#743,.T.);
#507=FACE_OUTER_BOUND('',#744,.T.);
#508=FACE_OUTER_BOUND('',#745,.T.);
#509=FACE_OUTER_BOUND('',#747,.T.);
#510=FACE_OUTER_BOUND('',#749,.T.);
#511=FACE_OUTER_BOUND('',#750,.T.);
#512=FACE_OUTER_BOUND('',#751,.T.);
#513=FACE_OUTER_BOUND('',#752,.T.);
#514=FACE_OUTER_BOUND('',#753,.T.);
#515=FACE_OUTER_BOUND('',#754,.T.);
#516=FACE_OUTER_BOUND('',#756,.T.);
#517=FACE_OUTER_BOUND('',#758,.T.);
#518=FACE_OUTER_BOUND('',#759,.T.);
#519=FACE_OUTER_BOUND('',#760,.T.);
#520=FACE_OUTER_BOUND('',#761,.T.);
#521=FACE_OUTER_BOUND('',#762,.T.);
#522=FACE_OUTER_BOUND('',#763,.T.);
#523=FACE_OUTER_BOUND('',#764,.T.);
#524=FACE_OUTER_BOUND('',#765,.T.);
#525=FACE_OUTER_BOUND('',#766,.T.);
#526=FACE_OUTER_BOUND('',#767,.T.);
#527=FACE_OUTER_BOUND('',#768,.T.);
#528=FACE_OUTER_BOUND('',#769,.T.);
#529=FACE_OUTER_BOUND('',#770,.T.);
#530=FACE_OUTER_BOUND('',#771,.T.);
#531=FACE_OUTER_BOUND('',#772,.T.);
#532=FACE_OUTER_BOUND('',#773,.T.);
#533=FACE_OUTER_BOUND('',#774,.T.);
#534=FACE_OUTER_BOUND('',#775,.T.);
#535=FACE_OUTER_BOUND('',#776,.T.);
#536=FACE_OUTER_BOUND('',#777,.T.);
#537=FACE_OUTER_BOUND('',#778,.T.);
#538=FACE_OUTER_BOUND('',#780,.T.);
#539=FACE_OUTER_BOUND('',#781,.T.);
#540=FACE_OUTER_BOUND('',#782,.T.);
#541=FACE_OUTER_BOUND('',#783,.T.);
#542=FACE_OUTER_BOUND('',#784,.T.);
#543=FACE_OUTER_BOUND('',#785,.T.);
#544=FACE_OUTER_BOUND('',#786,.T.);
#545=FACE_OUTER_BOUND('',#787,.T.);
#546=FACE_OUTER_BOUND('',#789,.T.);
#547=FACE_OUTER_BOUND('',#790,.T.);
#548=FACE_OUTER_BOUND('',#792,.T.);
#549=FACE_OUTER_BOUND('',#794,.T.);
#550=FACE_OUTER_BOUND('',#802,.T.);
#551=FACE_OUTER_BOUND('',#806,.T.);
#552=FACE_OUTER_BOUND('',#808,.T.);
#553=FACE_OUTER_BOUND('',#809,.T.);
#554=FACE_OUTER_BOUND('',#810,.T.);
#555=FACE_OUTER_BOUND('',#811,.T.);
#556=FACE_OUTER_BOUND('',#812,.T.);
#557=FACE_OUTER_BOUND('',#813,.T.);
#558=FACE_OUTER_BOUND('',#814,.T.);
#559=FACE_OUTER_BOUND('',#816,.T.);
#560=FACE_OUTER_BOUND('',#818,.T.);
#561=FACE_OUTER_BOUND('',#820,.T.);
#562=FACE_OUTER_BOUND('',#821,.T.);
#563=FACE_OUTER_BOUND('',#823,.T.);
#564=FACE_OUTER_BOUND('',#825,.T.);
#565=FACE_OUTER_BOUND('',#826,.T.);
#566=FACE_OUTER_BOUND('',#827,.T.);
#567=FACE_OUTER_BOUND('',#828,.T.);
#568=FACE_OUTER_BOUND('',#829,.T.);
#569=FACE_OUTER_BOUND('',#830,.T.);
#570=FACE_OUTER_BOUND('',#832,.T.);
#571=FACE_OUTER_BOUND('',#833,.T.);
#572=FACE_OUTER_BOUND('',#834,.T.);
#573=FACE_OUTER_BOUND('',#835,.T.);
#574=FACE_OUTER_BOUND('',#836,.T.);
#575=FACE_OUTER_BOUND('',#837,.T.);
#576=FACE_OUTER_BOUND('',#838,.T.);
#577=FACE_OUTER_BOUND('',#840,.T.);
#578=FACE_OUTER_BOUND('',#842,.T.);
#579=FACE_OUTER_BOUND('',#843,.T.);
#580=FACE_OUTER_BOUND('',#844,.T.);
#581=FACE_OUTER_BOUND('',#845,.T.);
#582=FACE_OUTER_BOUND('',#846,.T.);
#583=FACE_OUTER_BOUND('',#847,.T.);
#584=FACE_OUTER_BOUND('',#848,.T.);
#585=FACE_OUTER_BOUND('',#849,.T.);
#586=FACE_OUTER_BOUND('',#850,.T.);
#587=FACE_OUTER_BOUND('',#858,.T.);
#588=FACE_OUTER_BOUND('',#866,.T.);
#589=FACE_OUTER_BOUND('',#867,.T.);
#590=FACE_OUTER_BOUND('',#868,.T.);
#591=FACE_OUTER_BOUND('',#870,.T.);
#592=FACE_OUTER_BOUND('',#872,.T.);
#593=FACE_OUTER_BOUND('',#873,.T.);
#594=FACE_OUTER_BOUND('',#874,.T.);
#595=FACE_OUTER_BOUND('',#876,.T.);
#596=FACE_OUTER_BOUND('',#878,.T.);
#597=FACE_OUTER_BOUND('',#879,.T.);
#598=FACE_OUTER_BOUND('',#880,.T.);
#599=FACE_OUTER_BOUND('',#881,.T.);
#600=FACE_OUTER_BOUND('',#882,.T.);
#601=FACE_OUTER_BOUND('',#883,.T.);
#602=FACE_OUTER_BOUND('',#884,.T.);
#603=FACE_OUTER_BOUND('',#885,.T.);
#604=FACE_OUTER_BOUND('',#886,.T.);
#605=FACE_OUTER_BOUND('',#887,.T.);
#606=FACE_OUTER_BOUND('',#888,.T.);
#607=FACE_OUTER_BOUND('',#889,.T.);
#608=FACE_OUTER_BOUND('',#890,.T.);
#609=FACE_OUTER_BOUND('',#891,.T.);
#610=FACE_OUTER_BOUND('',#892,.T.);
#611=FACE_OUTER_BOUND('',#893,.T.);
#612=FACE_OUTER_BOUND('',#894,.T.);
#613=FACE_OUTER_BOUND('',#895,.T.);
#614=FACE_OUTER_BOUND('',#896,.T.);
#615=FACE_OUTER_BOUND('',#897,.T.);
#616=FACE_OUTER_BOUND('',#898,.T.);
#617=FACE_OUTER_BOUND('',#899,.T.);
#618=FACE_OUTER_BOUND('',#901,.T.);
#619=FACE_OUTER_BOUND('',#903,.T.);
#620=FACE_OUTER_BOUND('',#904,.T.);
#621=FACE_OUTER_BOUND('',#912,.T.);
#622=FACE_OUTER_BOUND('',#920,.T.);
#623=FACE_OUTER_BOUND('',#921,.T.);
#624=FACE_OUTER_BOUND('',#922,.T.);
#625=FACE_OUTER_BOUND('',#923,.T.);
#626=FACE_OUTER_BOUND('',#924,.T.);
#627=FACE_OUTER_BOUND('',#925,.T.);
#628=FACE_OUTER_BOUND('',#926,.T.);
#629=FACE_OUTER_BOUND('',#927,.T.);
#630=FACE_OUTER_BOUND('',#929,.T.);
#631=FACE_OUTER_BOUND('',#930,.T.);
#632=FACE_OUTER_BOUND('',#931,.T.);
#633=FACE_OUTER_BOUND('',#932,.T.);
#634=FACE_OUTER_BOUND('',#933,.T.);
#635=FACE_OUTER_BOUND('',#934,.T.);
#636=FACE_OUTER_BOUND('',#935,.T.);
#637=FACE_OUTER_BOUND('',#937,.T.);
#638=FACE_OUTER_BOUND('',#939,.T.);
#639=FACE_OUTER_BOUND('',#941,.T.);
#640=FACE_OUTER_BOUND('',#943,.T.);
#641=FACE_OUTER_BOUND('',#944,.T.);
#642=FACE_OUTER_BOUND('',#945,.T.);
#643=FACE_OUTER_BOUND('',#946,.T.);
#644=FACE_OUTER_BOUND('',#947,.T.);
#645=FACE_OUTER_BOUND('',#948,.T.);
#646=FACE_OUTER_BOUND('',#949,.T.);
#647=FACE_OUTER_BOUND('',#950,.T.);
#648=FACE_OUTER_BOUND('',#951,.T.);
#649=FACE_OUTER_BOUND('',#952,.T.);
#650=FACE_OUTER_BOUND('',#953,.T.);
#651=FACE_OUTER_BOUND('',#954,.T.);
#652=FACE_OUTER_BOUND('',#955,.T.);
#653=FACE_OUTER_BOUND('',#956,.T.);
#654=FACE_OUTER_BOUND('',#957,.T.);
#655=FACE_OUTER_BOUND('',#958,.T.);
#656=FACE_OUTER_BOUND('',#959,.T.);
#657=FACE_OUTER_BOUND('',#961,.T.);
#658=FACE_OUTER_BOUND('',#962,.T.);
#659=FACE_OUTER_BOUND('',#963,.T.);
#660=FACE_OUTER_BOUND('',#964,.T.);
#661=FACE_OUTER_BOUND('',#965,.T.);
#662=FACE_OUTER_BOUND('',#966,.T.);
#663=FACE_OUTER_BOUND('',#967,.T.);
#664=FACE_OUTER_BOUND('',#968,.T.);
#665=FACE_OUTER_BOUND('',#969,.T.);
#666=FACE_OUTER_BOUND('',#970,.T.);
#667=FACE_OUTER_BOUND('',#971,.T.);
#668=FACE_OUTER_BOUND('',#972,.T.);
#669=FACE_OUTER_BOUND('',#973,.T.);
#670=FACE_OUTER_BOUND('',#975,.T.);
#671=FACE_OUTER_BOUND('',#977,.T.);
#672=FACE_OUTER_BOUND('',#978,.T.);
#673=FACE_OUTER_BOUND('',#979,.T.);
#674=FACE_OUTER_BOUND('',#980,.T.);
#675=FACE_OUTER_BOUND('',#981,.T.);
#676=FACE_OUTER_BOUND('',#982,.T.);
#677=FACE_OUTER_BOUND('',#983,.T.);
#678=FACE_OUTER_BOUND('',#984,.T.);
#679=FACE_OUTER_BOUND('',#986,.T.);
#680=FACE_OUTER_BOUND('',#987,.T.);
#681=FACE_OUTER_BOUND('',#988,.T.);
#682=FACE_OUTER_BOUND('',#989,.T.);
#683=FACE_OUTER_BOUND('',#991,.T.);
#684=FACE_OUTER_BOUND('',#992,.T.);
#685=FACE_OUTER_BOUND('',#993,.T.);
#686=FACE_OUTER_BOUND('',#994,.T.);
#687=FACE_OUTER_BOUND('',#995,.T.);
#688=FACE_OUTER_BOUND('',#996,.T.);
#689=FACE_OUTER_BOUND('',#998,.T.);
#690=FACE_OUTER_BOUND('',#999,.T.);
#691=FACE_OUTER_BOUND('',#1000,.T.);
#692=FACE_OUTER_BOUND('',#1001,.T.);
#693=FACE_OUTER_BOUND('',#1002,.T.);
#694=FACE_OUTER_BOUND('',#1003,.T.);
#695=FACE_OUTER_BOUND('',#1004,.T.);
#696=FACE_OUTER_BOUND('',#1005,.T.);
#697=FACE_OUTER_BOUND('',#1006,.T.);
#698=FACE_OUTER_BOUND('',#1007,.T.);
#699=FACE_OUTER_BOUND('',#1008,.T.);
#700=FACE_OUTER_BOUND('',#1009,.T.);
#701=FACE_OUTER_BOUND('',#1010,.T.);
#702=FACE_OUTER_BOUND('',#1011,.T.);
#703=FACE_OUTER_BOUND('',#1012,.T.);
#704=FACE_OUTER_BOUND('',#1014,.T.);
#705=FACE_OUTER_BOUND('',#1016,.T.);
#706=FACE_OUTER_BOUND('',#1017,.T.);
#707=FACE_OUTER_BOUND('',#1018,.T.);
#708=FACE_OUTER_BOUND('',#1019,.T.);
#709=FACE_OUTER_BOUND('',#1020,.T.);
#710=FACE_OUTER_BOUND('',#1021,.T.);
#711=FACE_OUTER_BOUND('',#1022,.T.);
#712=FACE_OUTER_BOUND('',#1023,.T.);
#713=FACE_OUTER_BOUND('',#1024,.T.);
#714=FACE_OUTER_BOUND('',#1025,.T.);
#715=FACE_OUTER_BOUND('',#1027,.T.);
#716=FACE_OUTER_BOUND('',#1029,.T.);
#717=FACE_OUTER_BOUND('',#1030,.T.);
#718=FACE_OUTER_BOUND('',#1031,.T.);
#719=FACE_OUTER_BOUND('',#1032,.T.);
#720=FACE_OUTER_BOUND('',#1033,.T.);
#721=FACE_OUTER_BOUND('',#1034,.T.);
#722=FACE_OUTER_BOUND('',#1035,.T.);
#723=FACE_OUTER_BOUND('',#1036,.T.);
#724=FACE_OUTER_BOUND('',#1038,.T.);
#725=FACE_OUTER_BOUND('',#1039,.T.);
#726=FACE_OUTER_BOUND('',#1040,.T.);
#727=FACE_OUTER_BOUND('',#1041,.T.);
#728=EDGE_LOOP('',(#2458,#2459,#2460,#2461));
#729=EDGE_LOOP('',(#2462,#2463,#2464,#2465));
#730=EDGE_LOOP('',(#2466,#2467,#2468,#2469));
#731=EDGE_LOOP('',(#2470,#2471,#2472,#2473));
#732=EDGE_LOOP('',(#2474,#2475,#2476,#2477));
#733=EDGE_LOOP('',(#2478,#2479,#2480,#2481));
#734=EDGE_LOOP('',(#2482,#2483,#2484,#2485));
#735=EDGE_LOOP('',(#2486));
#736=EDGE_LOOP('',(#2487));
#737=EDGE_LOOP('',(#2488,#2489,#2490,#2491));
#738=EDGE_LOOP('',(#2492));
#739=EDGE_LOOP('',(#2493));
#740=EDGE_LOOP('',(#2494,#2495,#2496,#2497));
#741=EDGE_LOOP('',(#2498,#2499,#2500,#2501));
#742=EDGE_LOOP('',(#2502,#2503,#2504,#2505));
#743=EDGE_LOOP('',(#2506,#2507,#2508,#2509));
#744=EDGE_LOOP('',(#2510,#2511,#2512,#2513));
#745=EDGE_LOOP('',(#2514,#2515,#2516,#2517));
#746=EDGE_LOOP('',(#2518));
#747=EDGE_LOOP('',(#2519,#2520,#2521,#2522));
#748=EDGE_LOOP('',(#2523));
#749=EDGE_LOOP('',(#2524,#2525,#2526,#2527));
#750=EDGE_LOOP('',(#2528,#2529,#2530,#2531));
#751=EDGE_LOOP('',(#2532,#2533,#2534,#2535));
#752=EDGE_LOOP('',(#2536,#2537,#2538,#2539));
#753=EDGE_LOOP('',(#2540,#2541,#2542,#2543));
#754=EDGE_LOOP('',(#2544,#2545,#2546,#2547));
#755=EDGE_LOOP('',(#2548));
#756=EDGE_LOOP('',(#2549,#2550,#2551,#2552));
#757=EDGE_LOOP('',(#2553));
#758=EDGE_LOOP('',(#2554,#2555,#2556,#2557));
#759=EDGE_LOOP('',(#2558));
#760=EDGE_LOOP('',(#2559,#2560,#2561,#2562));
#761=EDGE_LOOP('',(#2563));
#762=EDGE_LOOP('',(#2564,#2565,#2566,#2567));
#763=EDGE_LOOP('',(#2568));
#764=EDGE_LOOP('',(#2569,#2570,#2571,#2572));
#765=EDGE_LOOP('',(#2573));
#766=EDGE_LOOP('',(#2574,#2575,#2576,#2577));
#767=EDGE_LOOP('',(#2578));
#768=EDGE_LOOP('',(#2579,#2580,#2581,#2582));
#769=EDGE_LOOP('',(#2583));
#770=EDGE_LOOP('',(#2584,#2585));
#771=EDGE_LOOP('',(#2586,#2587));
#772=EDGE_LOOP('',(#2588,#2589,#2590,#2591));
#773=EDGE_LOOP('',(#2592,#2593,#2594,#2595));
#774=EDGE_LOOP('',(#2596,#2597,#2598,#2599,#2600,#2601));
#775=EDGE_LOOP('',(#2602,#2603,#2604,#2605,#2606,#2607,#2608));
#776=EDGE_LOOP('',(#2609,#2610,#2611,#2612,#2613,#2614));
#777=EDGE_LOOP('',(#2615,#2616,#2617,#2618,#2619,#2620));
#778=EDGE_LOOP('',(#2621));
#779=EDGE_LOOP('',(#2622));
#780=EDGE_LOOP('',(#2623,#2624,#2625,#2626));
#781=EDGE_LOOP('',(#2627));
#782=EDGE_LOOP('',(#2628,#2629,#2630,#2631));
#783=EDGE_LOOP('',(#2632));
#784=EDGE_LOOP('',(#2633,#2634,#2635,#2636));
#785=EDGE_LOOP('',(#2637,#2638,#2639,#2640));
#786=EDGE_LOOP('',(#2641,#2642,#2643,#2644));
#787=EDGE_LOOP('',(#2645));
#788=EDGE_LOOP('',(#2646));
#789=EDGE_LOOP('',(#2647,#2648,#2649,#2650,#2651,#2652,#2653,#2654,#2655,
#2656,#2657,#2658));
#790=EDGE_LOOP('',(#2659));
#791=EDGE_LOOP('',(#2660));
#792=EDGE_LOOP('',(#2661,#2662,#2663,#2664,#2665,#2666,#2667,#2668,#2669));
#793=EDGE_LOOP('',(#2670,#2671));
#794=EDGE_LOOP('',(#2672));
#795=EDGE_LOOP('',(#2673));
#796=EDGE_LOOP('',(#2674));
#797=EDGE_LOOP('',(#2675));
#798=EDGE_LOOP('',(#2676));
#799=EDGE_LOOP('',(#2677));
#800=EDGE_LOOP('',(#2678));
#801=EDGE_LOOP('',(#2679));
#802=EDGE_LOOP('',(#2680));
#803=EDGE_LOOP('',(#2681));
#804=EDGE_LOOP('',(#2682));
#805=EDGE_LOOP('',(#2683));
#806=EDGE_LOOP('',(#2684));
#807=EDGE_LOOP('',(#2685));
#808=EDGE_LOOP('',(#2686,#2687,#2688,#2689));
#809=EDGE_LOOP('',(#2690));
#810=EDGE_LOOP('',(#2691,#2692,#2693,#2694));
#811=EDGE_LOOP('',(#2695));
#812=EDGE_LOOP('',(#2696,#2697,#2698,#2699));
#813=EDGE_LOOP('',(#2700,#2701,#2702,#2703));
#814=EDGE_LOOP('',(#2704));
#815=EDGE_LOOP('',(#2705));
#816=EDGE_LOOP('',(#2706));
#817=EDGE_LOOP('',(#2707));
#818=EDGE_LOOP('',(#2708));
#819=EDGE_LOOP('',(#2709));
#820=EDGE_LOOP('',(#2710,#2711,#2712,#2713));
#821=EDGE_LOOP('',(#2714));
#822=EDGE_LOOP('',(#2715));
#823=EDGE_LOOP('',(#2716));
#824=EDGE_LOOP('',(#2717));
#825=EDGE_LOOP('',(#2718,#2719,#2720,#2721));
#826=EDGE_LOOP('',(#2722,#2723,#2724,#2725));
#827=EDGE_LOOP('',(#2726,#2727,#2728,#2729));
#828=EDGE_LOOP('',(#2730));
#829=EDGE_LOOP('',(#2731,#2732,#2733,#2734));
#830=EDGE_LOOP('',(#2735));
#831=EDGE_LOOP('',(#2736));
#832=EDGE_LOOP('',(#2737));
#833=EDGE_LOOP('',(#2738,#2739,#2740,#2741));
#834=EDGE_LOOP('',(#2742));
#835=EDGE_LOOP('',(#2743));
#836=EDGE_LOOP('',(#2744,#2745,#2746,#2747));
#837=EDGE_LOOP('',(#2748,#2749,#2750,#2751));
#838=EDGE_LOOP('',(#2752));
#839=EDGE_LOOP('',(#2753));
#840=EDGE_LOOP('',(#2754));
#841=EDGE_LOOP('',(#2755));
#842=EDGE_LOOP('',(#2756,#2757,#2758,#2759));
#843=EDGE_LOOP('',(#2760,#2761,#2762,#2763));
#844=EDGE_LOOP('',(#2764,#2765,#2766,#2767));
#845=EDGE_LOOP('',(#2768,#2769,#2770,#2771));
#846=EDGE_LOOP('',(#2772,#2773,#2774,#2775));
#847=EDGE_LOOP('',(#2776,#2777,#2778,#2779));
#848=EDGE_LOOP('',(#2780,#2781,#2782,#2783));
#849=EDGE_LOOP('',(#2784,#2785,#2786,#2787));
#850=EDGE_LOOP('',(#2788));
#851=EDGE_LOOP('',(#2789));
#852=EDGE_LOOP('',(#2790));
#853=EDGE_LOOP('',(#2791));
#854=EDGE_LOOP('',(#2792));
#855=EDGE_LOOP('',(#2793));
#856=EDGE_LOOP('',(#2794));
#857=EDGE_LOOP('',(#2795));
#858=EDGE_LOOP('',(#2796));
#859=EDGE_LOOP('',(#2797));
#860=EDGE_LOOP('',(#2798));
#861=EDGE_LOOP('',(#2799));
#862=EDGE_LOOP('',(#2800));
#863=EDGE_LOOP('',(#2801));
#864=EDGE_LOOP('',(#2802));
#865=EDGE_LOOP('',(#2803));
#866=EDGE_LOOP('',(#2804,#2805,#2806,#2807));
#867=EDGE_LOOP('',(#2808,#2809,#2810,#2811));
#868=EDGE_LOOP('',(#2812));
#869=EDGE_LOOP('',(#2813));
#870=EDGE_LOOP('',(#2814));
#871=EDGE_LOOP('',(#2815));
#872=EDGE_LOOP('',(#2816,#2817,#2818,#2819));
#873=EDGE_LOOP('',(#2820,#2821,#2822,#2823));
#874=EDGE_LOOP('',(#2824));
#875=EDGE_LOOP('',(#2825));
#876=EDGE_LOOP('',(#2826));
#877=EDGE_LOOP('',(#2827));
#878=EDGE_LOOP('',(#2828,#2829));
#879=EDGE_LOOP('',(#2830,#2831,#2832,#2833));
#880=EDGE_LOOP('',(#2834,#2835,#2836,#2837));
#881=EDGE_LOOP('',(#2838,#2839));
#882=EDGE_LOOP('',(#2840,#2841));
#883=EDGE_LOOP('',(#2842,#2843,#2844,#2845));
#884=EDGE_LOOP('',(#2846,#2847));
#885=EDGE_LOOP('',(#2848,#2849,#2850,#2851));
#886=EDGE_LOOP('',(#2852,#2853));
#887=EDGE_LOOP('',(#2854,#2855,#2856,#2857));
#888=EDGE_LOOP('',(#2858,#2859,#2860,#2861));
#889=EDGE_LOOP('',(#2862,#2863));
#890=EDGE_LOOP('',(#2864,#2865,#2866,#2867,#2868,#2869,#2870,#2871,#2872,
#2873,#2874,#2875,#2876,#2877,#2878,#2879,#2880,#2881,#2882,#2883,#2884,
#2885,#2886,#2887,#2888,#2889,#2890,#2891));
#891=EDGE_LOOP('',(#2892,#2893,#2894,#2895));
#892=EDGE_LOOP('',(#2896,#2897,#2898,#2899));
#893=EDGE_LOOP('',(#2900,#2901,#2902,#2903));
#894=EDGE_LOOP('',(#2904,#2905,#2906,#2907));
#895=EDGE_LOOP('',(#2908,#2909,#2910,#2911));
#896=EDGE_LOOP('',(#2912,#2913,#2914,#2915));
#897=EDGE_LOOP('',(#2916,#2917,#2918,#2919));
#898=EDGE_LOOP('',(#2920,#2921,#2922,#2923));
#899=EDGE_LOOP('',(#2924));
#900=EDGE_LOOP('',(#2925));
#901=EDGE_LOOP('',(#2926));
#902=EDGE_LOOP('',(#2927));
#903=EDGE_LOOP('',(#2928,#2929,#2930,#2931));
#904=EDGE_LOOP('',(#2932));
#905=EDGE_LOOP('',(#2933));
#906=EDGE_LOOP('',(#2934));
#907=EDGE_LOOP('',(#2935));
#908=EDGE_LOOP('',(#2936));
#909=EDGE_LOOP('',(#2937));
#910=EDGE_LOOP('',(#2938));
#911=EDGE_LOOP('',(#2939,#2940,#2941,#2942,#2943,#2944,#2945,#2946,#2947,
#2948,#2949,#2950,#2951));
#912=EDGE_LOOP('',(#2952));
#913=EDGE_LOOP('',(#2953));
#914=EDGE_LOOP('',(#2954));
#915=EDGE_LOOP('',(#2955));
#916=EDGE_LOOP('',(#2956));
#917=EDGE_LOOP('',(#2957));
#918=EDGE_LOOP('',(#2958));
#919=EDGE_LOOP('',(#2959));
#920=EDGE_LOOP('',(#2960,#2961,#2962,#2963));
#921=EDGE_LOOP('',(#2964));
#922=EDGE_LOOP('',(#2965));
#923=EDGE_LOOP('',(#2966,#2967,#2968,#2969));
#924=EDGE_LOOP('',(#2970));
#925=EDGE_LOOP('',(#2971,#2972,#2973,#2974));
#926=EDGE_LOOP('',(#2975));
#927=EDGE_LOOP('',(#2976));
#928=EDGE_LOOP('',(#2977));
#929=EDGE_LOOP('',(#2978,#2979,#2980,#2981));
#930=EDGE_LOOP('',(#2982));
#931=EDGE_LOOP('',(#2983));
#932=EDGE_LOOP('',(#2984,#2985,#2986));
#933=EDGE_LOOP('',(#2987,#2988,#2989,#2990,#2991,#2992,#2993,#2994));
#934=EDGE_LOOP('',(#2995,#2996));
#935=EDGE_LOOP('',(#2997,#2998,#2999,#3000));
#936=EDGE_LOOP('',(#3001,#3002,#3003,#3004));
#937=EDGE_LOOP('',(#3005,#3006,#3007,#3008));
#938=EDGE_LOOP('',(#3009));
#939=EDGE_LOOP('',(#3010));
#940=EDGE_LOOP('',(#3011));
#941=EDGE_LOOP('',(#3012));
#942=EDGE_LOOP('',(#3013));
#943=EDGE_LOOP('',(#3014,#3015,#3016,#3017));
#944=EDGE_LOOP('',(#3018,#3019,#3020,#3021));
#945=EDGE_LOOP('',(#3022,#3023,#3024,#3025));
#946=EDGE_LOOP('',(#3026,#3027,#3028,#3029));
#947=EDGE_LOOP('',(#3030,#3031,#3032,#3033));
#948=EDGE_LOOP('',(#3034,#3035,#3036,#3037));
#949=EDGE_LOOP('',(#3038,#3039,#3040,#3041));
#950=EDGE_LOOP('',(#3042,#3043,#3044,#3045));
#951=EDGE_LOOP('',(#3046,#3047,#3048,#3049));
#952=EDGE_LOOP('',(#3050,#3051,#3052,#3053));
#953=EDGE_LOOP('',(#3054,#3055,#3056,#3057));
#954=EDGE_LOOP('',(#3058,#3059,#3060,#3061));
#955=EDGE_LOOP('',(#3062));
#956=EDGE_LOOP('',(#3063,#3064,#3065,#3066));
#957=EDGE_LOOP('',(#3067,#3068,#3069,#3070));
#958=EDGE_LOOP('',(#3071,#3072,#3073,#3074));
#959=EDGE_LOOP('',(#3075));
#960=EDGE_LOOP('',(#3076));
#961=EDGE_LOOP('',(#3077,#3078,#3079,#3080));
#962=EDGE_LOOP('',(#3081,#3082,#3083,#3084));
#963=EDGE_LOOP('',(#3085,#3086,#3087,#3088));
#964=EDGE_LOOP('',(#3089));
#965=EDGE_LOOP('',(#3090,#3091,#3092,#3093));
#966=EDGE_LOOP('',(#3094,#3095,#3096,#3097));
#967=EDGE_LOOP('',(#3098,#3099,#3100,#3101));
#968=EDGE_LOOP('',(#3102,#3103,#3104,#3105));
#969=EDGE_LOOP('',(#3106,#3107,#3108,#3109));
#970=EDGE_LOOP('',(#3110,#3111,#3112,#3113));
#971=EDGE_LOOP('',(#3114,#3115,#3116,#3117,#3118,#3119));
#972=EDGE_LOOP('',(#3120,#3121,#3122,#3123,#3124,#3125));
#973=EDGE_LOOP('',(#3126,#3127,#3128,#3129,#3130,#3131));
#974=EDGE_LOOP('',(#3132));
#975=EDGE_LOOP('',(#3133,#3134,#3135,#3136,#3137,#3138));
#976=EDGE_LOOP('',(#3139));
#977=EDGE_LOOP('',(#3140,#3141,#3142,#3143));
#978=EDGE_LOOP('',(#3144,#3145,#3146,#3147));
#979=EDGE_LOOP('',(#3148,#3149,#3150,#3151));
#980=EDGE_LOOP('',(#3152,#3153,#3154,#3155));
#981=EDGE_LOOP('',(#3156,#3157,#3158,#3159));
#982=EDGE_LOOP('',(#3160,#3161,#3162,#3163));
#983=EDGE_LOOP('',(#3164,#3165,#3166,#3167));
#984=EDGE_LOOP('',(#3168));
#985=EDGE_LOOP('',(#3169));
#986=EDGE_LOOP('',(#3170,#3171,#3172,#3173));
#987=EDGE_LOOP('',(#3174,#3175,#3176,#3177));
#988=EDGE_LOOP('',(#3178,#3179,#3180,#3181));
#989=EDGE_LOOP('',(#3182));
#990=EDGE_LOOP('',(#3183));
#991=EDGE_LOOP('',(#3184,#3185,#3186,#3187));
#992=EDGE_LOOP('',(#3188));
#993=EDGE_LOOP('',(#3189,#3190,#3191,#3192));
#994=EDGE_LOOP('',(#3193,#3194,#3195,#3196));
#995=EDGE_LOOP('',(#3197,#3198,#3199,#3200));
#996=EDGE_LOOP('',(#3201));
#997=EDGE_LOOP('',(#3202));
#998=EDGE_LOOP('',(#3203,#3204,#3205,#3206));
#999=EDGE_LOOP('',(#3207,#3208,#3209,#3210));
#1000=EDGE_LOOP('',(#3211,#3212,#3213,#3214));
#1001=EDGE_LOOP('',(#3215));
#1002=EDGE_LOOP('',(#3216,#3217,#3218,#3219));
#1003=EDGE_LOOP('',(#3220,#3221,#3222,#3223));
#1004=EDGE_LOOP('',(#3224,#3225,#3226,#3227));
#1005=EDGE_LOOP('',(#3228,#3229,#3230,#3231));
#1006=EDGE_LOOP('',(#3232,#3233,#3234,#3235));
#1007=EDGE_LOOP('',(#3236,#3237,#3238,#3239));
#1008=EDGE_LOOP('',(#3240,#3241,#3242,#3243,#3244,#3245));
#1009=EDGE_LOOP('',(#3246,#3247,#3248,#3249,#3250,#3251));
#1010=EDGE_LOOP('',(#3252,#3253,#3254,#3255));
#1011=EDGE_LOOP('',(#3256,#3257,#3258,#3259));
#1012=EDGE_LOOP('',(#3260));
#1013=EDGE_LOOP('',(#3261));
#1014=EDGE_LOOP('',(#3262));
#1015=EDGE_LOOP('',(#3263));
#1016=EDGE_LOOP('',(#3264,#3265,#3266,#3267,#3268,#3269,#3270,#3271,#3272));
#1017=EDGE_LOOP('',(#3273,#3274,#3275,#3276,#3277,#3278,#3279,#3280,#3281));
#1018=EDGE_LOOP('',(#3282,#3283,#3284,#3285));
#1019=EDGE_LOOP('',(#3286,#3287,#3288,#3289));
#1020=EDGE_LOOP('',(#3290,#3291,#3292,#3293));
#1021=EDGE_LOOP('',(#3294,#3295,#3296,#3297));
#1022=EDGE_LOOP('',(#3298,#3299,#3300,#3301));
#1023=EDGE_LOOP('',(#3302,#3303,#3304,#3305));
#1024=EDGE_LOOP('',(#3306,#3307,#3308,#3309));
#1025=EDGE_LOOP('',(#3310));
#1026=EDGE_LOOP('',(#3311));
#1027=EDGE_LOOP('',(#3312));
#1028=EDGE_LOOP('',(#3313));
#1029=EDGE_LOOP('',(#3314,#3315,#3316,#3317));
#1030=EDGE_LOOP('',(#3318,#3319,#3320,#3321));
#1031=EDGE_LOOP('',(#3322,#3323,#3324,#3325));
#1032=EDGE_LOOP('',(#3326,#3327,#3328,#3329));
#1033=EDGE_LOOP('',(#3330,#3331,#3332,#3333));
#1034=EDGE_LOOP('',(#3334,#3335,#3336,#3337));
#1035=EDGE_LOOP('',(#3338,#3339,#3340,#3341,#3342,#3343));
#1036=EDGE_LOOP('',(#3344));
#1037=EDGE_LOOP('',(#3345,#3346,#3347,#3348,#3349,#3350));
#1038=EDGE_LOOP('',(#3351,#3352,#3353,#3354));
#1039=EDGE_LOOP('',(#3355,#3356,#3357,#3358));
#1040=EDGE_LOOP('',(#3359,#3360,#3361,#3362));
#1041=EDGE_LOOP('',(#3363));
#1042=LINE('',#5626,#1286);
#1043=LINE('',#5632,#1287);
#1044=LINE('',#5637,#1288);
#1045=LINE('',#5639,#1289);
#1046=LINE('',#5641,#1290);
#1047=LINE('',#5642,#1291);
#1048=LINE('',#5645,#1292);
#1049=LINE('',#5647,#1293);
#1050=LINE('',#5648,#1294);
#1051=LINE('',#5651,#1295);
#1052=LINE('',#5653,#1296);
#1053=LINE('',#5654,#1297);
#1054=LINE('',#5656,#1298);
#1055=LINE('',#5657,#1299);
#1056=LINE('',#5665,#1300);
#1057=LINE('',#5670,#1301);
#1058=LINE('',#5672,#1302);
#1059=LINE('',#5674,#1303);
#1060=LINE('',#5675,#1304);
#1061=LINE('',#5678,#1305);
#1062=LINE('',#5680,#1306);
#1063=LINE('',#5681,#1307);
#1064=LINE('',#5684,#1308);
#1065=LINE('',#5686,#1309);
#1066=LINE('',#5687,#1310);
#1067=LINE('',#5689,#1311);
#1068=LINE('',#5690,#1312);
#1069=LINE('',#5698,#1313);
#1070=LINE('',#5703,#1314);
#1071=LINE('',#5705,#1315);
#1072=LINE('',#5707,#1316);
#1073=LINE('',#5708,#1317);
#1074=LINE('',#5711,#1318);
#1075=LINE('',#5713,#1319);
#1076=LINE('',#5714,#1320);
#1077=LINE('',#5717,#1321);
#1078=LINE('',#5719,#1322);
#1079=LINE('',#5720,#1323);
#1080=LINE('',#5722,#1324);
#1081=LINE('',#5723,#1325);
#1082=LINE('',#5731,#1326);
#1083=LINE('',#5738,#1327);
#1084=LINE('',#5745,#1328);
#1085=LINE('',#5752,#1329);
#1086=LINE('',#5759,#1330);
#1087=LINE('',#5766,#1331);
#1088=LINE('',#5814,#1332);
#1089=LINE('',#5817,#1333);
#1090=LINE('',#5819,#1334);
#1091=LINE('',#5821,#1335);
#1092=LINE('',#5824,#1336);
#1093=LINE('',#5866,#1337);
#1094=LINE('',#5887,#1338);
#1095=LINE('',#5888,#1339);
#1096=LINE('',#5911,#1340);
#1097=LINE('',#5956,#1341);
#1098=LINE('',#5963,#1342);
#1099=LINE('',#5970,#1343);
#1100=LINE('',#5976,#1344);
#1101=LINE('',#5983,#1345);
#1102=LINE('',#5989,#1346);
#1103=LINE('',#5991,#1347);
#1104=LINE('',#5997,#1348);
#1105=LINE('',#5999,#1349);
#1106=LINE('',#6011,#1350);
#1107=LINE('',#6017,#1351);
#1108=LINE('',#6024,#1352);
#1109=LINE('',#6030,#1353);
#1110=LINE('',#6043,#1354);
#1111=LINE('',#6055,#1355);
#1112=LINE('',#6058,#1356);
#1113=LINE('',#6061,#1357);
#1114=LINE('',#6067,#1358);
#1115=LINE('',#6815,#1359);
#1116=LINE('',#6821,#1360);
#1117=LINE('',#6830,#1361);
#1118=LINE('',#6836,#1362);
#1119=LINE('',#6842,#1363);
#1120=LINE('',#6848,#1364);
#1121=LINE('',#6854,#1365);
#1122=LINE('',#6860,#1366);
#1123=LINE('',#6866,#1367);
#1124=LINE('',#6872,#1368);
#1125=LINE('',#6881,#1369);
#1126=LINE('',#6887,#1370);
#1127=LINE('',#6897,#1371);
#1128=LINE('',#6901,#1372);
#1129=LINE('',#6913,#1373);
#1130=LINE('',#6916,#1374);
#1131=LINE('',#6920,#1375);
#1132=LINE('',#6924,#1376);
#1133=LINE('',#6935,#1377);
#1134=LINE('',#6938,#1378);
#1135=LINE('',#6946,#1379);
#1136=LINE('',#6949,#1380);
#1137=LINE('',#6957,#1381);
#1138=LINE('',#6960,#1382);
#1139=LINE('',#6964,#1383);
#1140=LINE('',#6968,#1384);
#1141=LINE('',#6976,#1385);
#1142=LINE('',#6988,#1386);
#1143=LINE('',#6994,#1387);
#1144=LINE('',#7000,#1388);
#1145=LINE('',#7006,#1389);
#1146=LINE('',#7012,#1390);
#1147=LINE('',#7018,#1391);
#1148=LINE('',#7024,#1392);
#1149=LINE('',#7030,#1393);
#1150=LINE('',#7038,#1394);
#1151=LINE('',#7835,#1395);
#1152=LINE('',#7842,#1396);
#1153=LINE('',#7851,#1397);
#1154=LINE('',#7859,#1398);
#1155=LINE('',#7888,#1399);
#1156=LINE('',#7924,#1400);
#1157=LINE('',#7929,#1401);
#1158=LINE('',#7935,#1402);
#1159=LINE('',#7943,#1403);
#1160=LINE('',#7945,#1404);
#1161=LINE('',#7947,#1405);
#1162=LINE('',#7948,#1406);
#1163=LINE('',#7951,#1407);
#1164=LINE('',#7953,#1408);
#1165=LINE('',#7954,#1409);
#1166=LINE('',#7957,#1410);
#1167=LINE('',#7959,#1411);
#1168=LINE('',#7960,#1412);
#1169=LINE('',#7962,#1413);
#1170=LINE('',#7963,#1414);
#1171=LINE('',#7970,#1415);
#1172=LINE('',#7972,#1416);
#1173=LINE('',#7974,#1417);
#1174=LINE('',#7975,#1418);
#1175=LINE('',#7978,#1419);
#1176=LINE('',#7980,#1420);
#1177=LINE('',#7981,#1421);
#1178=LINE('',#7984,#1422);
#1179=LINE('',#7986,#1423);
#1180=LINE('',#7987,#1424);
#1181=LINE('',#7989,#1425);
#1182=LINE('',#7990,#1426);
#1183=LINE('',#8000,#1427);
#1184=LINE('',#8004,#1428);
#1185=LINE('',#8008,#1429);
#1186=LINE('',#8015,#1430);
#1187=LINE('',#8019,#1431);
#1188=LINE('',#8023,#1432);
#1189=LINE('',#8028,#1433);
#1190=LINE('',#8030,#1434);
#1191=LINE('',#8032,#1435);
#1192=LINE('',#8033,#1436);
#1193=LINE('',#8036,#1437);
#1194=LINE('',#8038,#1438);
#1195=LINE('',#8039,#1439);
#1196=LINE('',#8042,#1440);
#1197=LINE('',#8044,#1441);
#1198=LINE('',#8045,#1442);
#1199=LINE('',#8048,#1443);
#1200=LINE('',#8050,#1444);
#1201=LINE('',#8051,#1445);
#1202=LINE('',#8054,#1446);
#1203=LINE('',#8056,#1447);
#1204=LINE('',#8057,#1448);
#1205=LINE('',#8059,#1449);
#1206=LINE('',#8060,#1450);
#1207=LINE('',#8067,#1451);
#1208=LINE('',#8069,#1452);
#1209=LINE('',#8071,#1453);
#1210=LINE('',#8073,#1454);
#1211=LINE('',#8075,#1455);
#1212=LINE('',#8076,#1456);
#1213=LINE('',#8082,#1457);
#1214=LINE('',#8084,#1458);
#1215=LINE('',#8086,#1459);
#1216=LINE('',#8088,#1460);
#1217=LINE('',#8090,#1461);
#1218=LINE('',#8091,#1462);
#1219=LINE('',#8095,#1463);
#1220=LINE('',#8096,#1464);
#1221=LINE('',#8098,#1465);
#1222=LINE('',#8100,#1466);
#1223=LINE('',#8102,#1467);
#1224=LINE('',#8104,#1468);
#1225=LINE('',#8108,#1469);
#1226=LINE('',#8116,#1470);
#1227=LINE('',#8120,#1471);
#1228=LINE('',#8124,#1472);
#1229=LINE('',#8129,#1473);
#1230=LINE('',#8137,#1474);
#1231=LINE('',#8141,#1475);
#1232=LINE('',#8145,#1476);
#1233=LINE('',#8152,#1477);
#1234=LINE('',#8156,#1478);
#1235=LINE('',#8160,#1479);
#1236=LINE('',#8165,#1480);
#1237=LINE('',#8167,#1481);
#1238=LINE('',#8169,#1482);
#1239=LINE('',#8170,#1483);
#1240=LINE('',#8173,#1484);
#1241=LINE('',#8175,#1485);
#1242=LINE('',#8176,#1486);
#1243=LINE('',#8179,#1487);
#1244=LINE('',#8181,#1488);
#1245=LINE('',#8182,#1489);
#1246=LINE('',#8185,#1490);
#1247=LINE('',#8187,#1491);
#1248=LINE('',#8188,#1492);
#1249=LINE('',#8191,#1493);
#1250=LINE('',#8193,#1494);
#1251=LINE('',#8194,#1495);
#1252=LINE('',#8196,#1496);
#1253=LINE('',#8197,#1497);
#1254=LINE('',#8205,#1498);
#1255=LINE('',#8211,#1499);
#1256=LINE('',#8227,#1500);
#1257=LINE('',#8248,#1501);
#1258=LINE('',#8273,#1502);
#1259=LINE('',#8274,#1503);
#1260=LINE('',#8276,#1504);
#1261=LINE('',#8278,#1505);
#1262=LINE('',#8283,#1506);
#1263=LINE('',#8286,#1507);
#1264=LINE('',#8288,#1508);
#1265=LINE('',#8296,#1509);
#1266=LINE('',#8298,#1510);
#1267=LINE('',#8300,#1511);
#1268=LINE('',#8301,#1512);
#1269=LINE('',#8304,#1513);
#1270=LINE('',#8306,#1514);
#1271=LINE('',#8307,#1515);
#1272=LINE('',#8310,#1516);
#1273=LINE('',#8312,#1517);
#1274=LINE('',#8313,#1518);
#1275=LINE('',#8316,#1519);
#1276=LINE('',#8318,#1520);
#1277=LINE('',#8319,#1521);
#1278=LINE('',#8322,#1522);
#1279=LINE('',#8324,#1523);
#1280=LINE('',#8325,#1524);
#1281=LINE('',#8327,#1525);
#1282=LINE('',#8328,#1526);
#1283=LINE('',#8336,#1527);
#1284=LINE('',#8340,#1528);
#1285=LINE('',#8344,#1529);
#1286=VECTOR('',#4444,0.225);
#1287=VECTOR('',#4451,0.225);
#1288=VECTOR('',#4456,1.);
#1289=VECTOR('',#4457,1.);
#1290=VECTOR('',#4458,1.);
#1291=VECTOR('',#4459,1.);
#1292=VECTOR('',#4462,1.);
#1293=VECTOR('',#4463,1.);
#1294=VECTOR('',#4464,1.);
#1295=VECTOR('',#4467,1.);
#1296=VECTOR('',#4468,1.);
#1297=VECTOR('',#4469,1.);
#1298=VECTOR('',#4472,1.);
#1299=VECTOR('',#4473,1.);
#1300=VECTOR('',#4484,0.225);
#1301=VECTOR('',#4489,1.);
#1302=VECTOR('',#4490,1.);
#1303=VECTOR('',#4491,1.);
#1304=VECTOR('',#4492,1.);
#1305=VECTOR('',#4495,1.);
#1306=VECTOR('',#4496,1.);
#1307=VECTOR('',#4497,1.);
#1308=VECTOR('',#4500,1.);
#1309=VECTOR('',#4501,1.);
#1310=VECTOR('',#4502,1.);
#1311=VECTOR('',#4505,1.);
#1312=VECTOR('',#4506,1.);
#1313=VECTOR('',#4517,0.225);
#1314=VECTOR('',#4522,1.);
#1315=VECTOR('',#4523,1.);
#1316=VECTOR('',#4524,1.);
#1317=VECTOR('',#4525,1.);
#1318=VECTOR('',#4528,1.);
#1319=VECTOR('',#4529,1.);
#1320=VECTOR('',#4530,1.);
#1321=VECTOR('',#4533,1.);
#1322=VECTOR('',#4534,1.);
#1323=VECTOR('',#4535,1.);
#1324=VECTOR('',#4538,1.);
#1325=VECTOR('',#4539,1.);
#1326=VECTOR('',#4550,0.21);
#1327=VECTOR('',#4559,0.21);
#1328=VECTOR('',#4568,0.21);
#1329=VECTOR('',#4577,0.21);
#1330=VECTOR('',#4586,0.21);
#1331=VECTOR('',#4595,0.21);
#1332=VECTOR('',#4610,1.);
#1333=VECTOR('',#4613,1.);
#1334=VECTOR('',#4616,1.);
#1335=VECTOR('',#4619,1.);
#1336=VECTOR('',#4622,0.685);
#1337=VECTOR('',#4627,0.4);
#1338=VECTOR('',#4628,1.);
#1339=VECTOR('',#4629,1.);
#1340=VECTOR('',#4634,0.8);
#1341=VECTOR('',#4639,0.685);
#1342=VECTOR('',#4648,0.165);
#1343=VECTOR('',#4657,0.165);
#1344=VECTOR('',#4666,0.925);
#1345=VECTOR('',#4675,0.6);
#1346=VECTOR('',#4684,2.5);
#1347=VECTOR('',#4685,2.5);
#1348=VECTOR('',#4694,4.);
#1349=VECTOR('',#4695,4.);
#1350=VECTOR('',#4712,1.3);
#1351=VECTOR('',#4721,1.);
#1352=VECTOR('',#4730,0.2);
#1353=VECTOR('',#4737,0.6);
#1354=VECTOR('',#4756,0.4);
#1355=VECTOR('',#4771,0.4);
#1356=VECTOR('',#4774,0.15);
#1357=VECTOR('',#4779,0.15);
#1358=VECTOR('',#4786,0.4);
#1359=VECTOR('',#4809,0.16);
#1360=VECTOR('',#4816,2.2);
#1361=VECTOR('',#4829,0.275);
#1362=VECTOR('',#4836,0.275);
#1363=VECTOR('',#4843,0.275);
#1364=VECTOR('',#4850,0.275);
#1365=VECTOR('',#4857,0.275);
#1366=VECTOR('',#4864,0.275);
#1367=VECTOR('',#4871,0.16);
#1368=VECTOR('',#4878,4.);
#1369=VECTOR('',#4891,0.41);
#1370=VECTOR('',#4898,0.6);
#1371=VECTOR('',#4911,0.16);
#1372=VECTOR('',#4916,2.2);
#1373=VECTOR('',#4933,1.);
#1374=VECTOR('',#4936,1.);
#1375=VECTOR('',#4939,1.);
#1376=VECTOR('',#4942,1.);
#1377=VECTOR('',#4957,1.);
#1378=VECTOR('',#4960,1.);
#1379=VECTOR('',#4969,1.);
#1380=VECTOR('',#4972,1.);
#1381=VECTOR('',#4981,1.);
#1382=VECTOR('',#4984,1.);
#1383=VECTOR('',#4987,1.);
#1384=VECTOR('',#4990,1.);
#1385=VECTOR('',#5001,3.);
#1386=VECTOR('',#5020,0.275);
#1387=VECTOR('',#5027,0.275);
#1388=VECTOR('',#5034,0.275);
#1389=VECTOR('',#5041,0.275);
#1390=VECTOR('',#5048,0.275);
#1391=VECTOR('',#5055,0.275);
#1392=VECTOR('',#5062,0.34);
#1393=VECTOR('',#5069,2.5);
#1394=VECTOR('',#5080,4.);
#1395=VECTOR('',#5103,0.6);
#1396=VECTOR('',#5112,1.2);
#1397=VECTOR('',#5125,0.4);
#1398=VECTOR('',#5136,1.);
#1399=VECTOR('',#5145,0.165);
#1400=VECTOR('',#5148,1.);
#1401=VECTOR('',#5153,0.4);
#1402=VECTOR('',#5160,1.5);
#1403=VECTOR('',#5171,1.);
#1404=VECTOR('',#5172,1.);
#1405=VECTOR('',#5173,1.);
#1406=VECTOR('',#5174,1.);
#1407=VECTOR('',#5177,1.);
#1408=VECTOR('',#5178,1.);
#1409=VECTOR('',#5179,1.);
#1410=VECTOR('',#5182,1.);
#1411=VECTOR('',#5183,1.);
#1412=VECTOR('',#5184,1.);
#1413=VECTOR('',#5187,1.);
#1414=VECTOR('',#5188,1.);
#1415=VECTOR('',#5197,1.);
#1416=VECTOR('',#5198,1.);
#1417=VECTOR('',#5199,1.);
#1418=VECTOR('',#5200,1.);
#1419=VECTOR('',#5203,1.);
#1420=VECTOR('',#5204,1.);
#1421=VECTOR('',#5205,1.);
#1422=VECTOR('',#5208,1.);
#1423=VECTOR('',#5209,1.);
#1424=VECTOR('',#5210,1.);
#1425=VECTOR('',#5213,1.);
#1426=VECTOR('',#5214,1.);
#1427=VECTOR('',#5229,0.325);
#1428=VECTOR('',#5234,0.35);
#1429=VECTOR('',#5239,0.335);
#1430=VECTOR('',#5248,0.21);
#1431=VECTOR('',#5253,0.2);
#1432=VECTOR('',#5258,0.18);
#1433=VECTOR('',#5263,1.);
#1434=VECTOR('',#5264,1.);
#1435=VECTOR('',#5265,1.);
#1436=VECTOR('',#5266,1.);
#1437=VECTOR('',#5269,1.);
#1438=VECTOR('',#5270,1.);
#1439=VECTOR('',#5271,1.);
#1440=VECTOR('',#5274,1.);
#1441=VECTOR('',#5275,1.);
#1442=VECTOR('',#5276,1.);
#1443=VECTOR('',#5279,1.);
#1444=VECTOR('',#5280,1.);
#1445=VECTOR('',#5281,1.);
#1446=VECTOR('',#5284,1.);
#1447=VECTOR('',#5285,1.);
#1448=VECTOR('',#5286,1.);
#1449=VECTOR('',#5289,1.);
#1450=VECTOR('',#5290,1.);
#1451=VECTOR('',#5299,1.);
#1452=VECTOR('',#5300,1.);
#1453=VECTOR('',#5301,1.);
#1454=VECTOR('',#5302,1.);
#1455=VECTOR('',#5303,1.);
#1456=VECTOR('',#5304,1.);
#1457=VECTOR('',#5309,1.);
#1458=VECTOR('',#5310,1.);
#1459=VECTOR('',#5311,1.);
#1460=VECTOR('',#5312,1.);
#1461=VECTOR('',#5313,1.);
#1462=VECTOR('',#5314,1.);
#1463=VECTOR('',#5319,1.);
#1464=VECTOR('',#5320,1.);
#1465=VECTOR('',#5323,1.);
#1466=VECTOR('',#5326,1.);
#1467=VECTOR('',#5329,1.);
#1468=VECTOR('',#5332,1.);
#1469=VECTOR('',#5337,0.685);
#1470=VECTOR('',#5348,0.645);
#1471=VECTOR('',#5353,0.685);
#1472=VECTOR('',#5358,0.645);
#1473=VECTOR('',#5365,0.46);
#1474=VECTOR('',#5376,0.4);
#1475=VECTOR('',#5381,0.425);
#1476=VECTOR('',#5386,0.41);
#1477=VECTOR('',#5395,0.26);
#1478=VECTOR('',#5400,0.25);
#1479=VECTOR('',#5405,0.225);
#1480=VECTOR('',#5410,1.);
#1481=VECTOR('',#5411,1.);
#1482=VECTOR('',#5412,1.);
#1483=VECTOR('',#5413,1.);
#1484=VECTOR('',#5416,1.);
#1485=VECTOR('',#5417,1.);
#1486=VECTOR('',#5418,1.);
#1487=VECTOR('',#5421,1.);
#1488=VECTOR('',#5422,1.);
#1489=VECTOR('',#5423,1.);
#1490=VECTOR('',#5426,1.);
#1491=VECTOR('',#5427,1.);
#1492=VECTOR('',#5428,1.);
#1493=VECTOR('',#5431,1.);
#1494=VECTOR('',#5432,1.);
#1495=VECTOR('',#5433,1.);
#1496=VECTOR('',#5436,1.);
#1497=VECTOR('',#5437,1.);
#1498=VECTOR('',#5448,0.42);
#1499=VECTOR('',#5455,0.8);
#1500=VECTOR('',#5466,0.734027674973257);
#1501=VECTOR('',#5473,0.734027674973257);
#1502=VECTOR('',#5476,1.);
#1503=VECTOR('',#5477,1.);
#1504=VECTOR('',#5480,1.);
#1505=VECTOR('',#5483,1.);
#1506=VECTOR('',#5488,0.4);
#1507=VECTOR('',#5493,1.);
#1508=VECTOR('',#5496,1.);
#1509=VECTOR('',#5507,1.);
#1510=VECTOR('',#5508,1.);
#1511=VECTOR('',#5509,1.);
#1512=VECTOR('',#5510,1.);
#1513=VECTOR('',#5513,1.);
#1514=VECTOR('',#5514,1.);
#1515=VECTOR('',#5515,1.);
#1516=VECTOR('',#5518,1.);
#1517=VECTOR('',#5519,1.);
#1518=VECTOR('',#5520,1.);
#1519=VECTOR('',#5523,1.);
#1520=VECTOR('',#5524,1.);
#1521=VECTOR('',#5525,1.);
#1522=VECTOR('',#5528,1.);
#1523=VECTOR('',#5529,1.);
#1524=VECTOR('',#5530,1.);
#1525=VECTOR('',#5533,1.);
#1526=VECTOR('',#5534,1.);
#1527=VECTOR('',#5545,0.185);
#1528=VECTOR('',#5550,0.2);
#1529=VECTOR('',#5555,0.1625);
#1530=CIRCLE('',#3969,0.225);
#1531=CIRCLE('',#3970,0.225);
#1532=CIRCLE('',#3972,0.225);
#1533=CIRCLE('',#3973,0.225);
#1534=CIRCLE('',#3982,0.225);
#1535=CIRCLE('',#3983,0.225);
#1536=CIRCLE('',#3992,0.225);
#1537=CIRCLE('',#3993,0.225);
#1538=CIRCLE('',#4002,0.21);
#1539=CIRCLE('',#4003,0.21);
#1540=CIRCLE('',#4006,0.21);
#1541=CIRCLE('',#4007,0.21);
#1542=CIRCLE('',#4010,0.21);
#1543=CIRCLE('',#4011,0.21);
#1544=CIRCLE('',#4014,0.21);
#1545=CIRCLE('',#4015,0.21);
#1546=CIRCLE('',#4018,0.21);
#1547=CIRCLE('',#4019,0.21);
#1548=CIRCLE('',#4022,0.21);
#1549=CIRCLE('',#4023,0.21);
#1550=CIRCLE('',#4026,0.4);
#1551=CIRCLE('',#4028,0.4);
#1552=CIRCLE('',#4030,0.685);
#1553=CIRCLE('',#4032,0.685);
#1554=CIRCLE('',#4035,0.4);
#1555=CIRCLE('',#4037,0.8);
#1556=CIRCLE('',#4038,0.8);
#1557=CIRCLE('',#4040,0.685);
#1558=CIRCLE('',#4043,0.165);
#1559=CIRCLE('',#4044,0.165);
#1560=CIRCLE('',#4047,0.165);
#1561=CIRCLE('',#4048,0.165);
#1562=CIRCLE('',#4051,0.925);
#1563=CIRCLE('',#4052,0.925);
#1564=CIRCLE('',#4055,0.6);
#1565=CIRCLE('',#4056,0.6);
#1566=CIRCLE('',#4059,2.5);
#1567=CIRCLE('',#4060,2.5);
#1568=CIRCLE('',#4063,4.);
#1569=CIRCLE('',#4064,4.);
#1570=CIRCLE('',#4069,1.3);
#1571=CIRCLE('',#4070,1.);
#1572=CIRCLE('',#4072,1.3);
#1573=CIRCLE('',#4075,1.);
#1574=CIRCLE('',#4079,0.2);
#1575=CIRCLE('',#4080,0.2);
#1576=CIRCLE('',#4082,0.6);
#1577=CIRCLE('',#4083,0.6);
#1578=CIRCLE('',#4088,0.4);
#1579=CIRCLE('',#4089,0.15);
#1580=CIRCLE('',#4091,0.4);
#1581=CIRCLE('',#4093,0.4);
#1582=CIRCLE('',#4094,0.15);
#1583=CIRCLE('',#4096,0.4);
#1584=CIRCLE('',#4097,0.15);
#1585=CIRCLE('',#4100,0.15);
#1586=CIRCLE('',#4104,0.4);
#1587=CIRCLE('',#4105,0.4);
#1588=CIRCLE('',#4109,0.03);
#1589=CIRCLE('',#4110,0.03);
#1590=CIRCLE('',#4115,0.16);
#1591=CIRCLE('',#4116,0.16);
#1592=CIRCLE('',#4118,2.2);
#1593=CIRCLE('',#4119,2.2);
#1594=CIRCLE('',#4124,0.275);
#1595=CIRCLE('',#4125,0.275);
#1596=CIRCLE('',#4127,0.275);
#1597=CIRCLE('',#4128,0.275);
#1598=CIRCLE('',#4130,0.275);
#1599=CIRCLE('',#4131,0.275);
#1600=CIRCLE('',#4133,0.275);
#1601=CIRCLE('',#4134,0.275);
#1602=CIRCLE('',#4136,0.275);
#1603=CIRCLE('',#4137,0.275);
#1604=CIRCLE('',#4139,0.275);
#1605=CIRCLE('',#4140,0.275);
#1606=CIRCLE('',#4142,0.16);
#1607=CIRCLE('',#4143,0.16);
#1608=CIRCLE('',#4145,4.);
#1609=CIRCLE('',#4146,4.);
#1610=CIRCLE('',#4151,0.41);
#1611=CIRCLE('',#4152,0.41);
#1612=CIRCLE('',#4154,0.6);
#1613=CIRCLE('',#4155,0.6);
#1614=CIRCLE('',#4158,2.2);
#1615=CIRCLE('',#4160,0.16);
#1616=CIRCLE('',#4161,0.16);
#1617=CIRCLE('',#4163,2.2);
#1618=CIRCLE('',#4168,3.);
#1619=CIRCLE('',#4169,0.525);
#1620=CIRCLE('',#4171,0.525);
#1621=CIRCLE('',#4173,0.525);
#1622=CIRCLE('',#4174,0.525);
#1623=CIRCLE('',#4176,3.);
#1624=CIRCLE('',#4178,3.);
#1625=CIRCLE('',#4179,0.525);
#1626=CIRCLE('',#4181,0.525);
#1627=CIRCLE('',#4183,3.);
#1628=CIRCLE('',#4184,0.525);
#1629=CIRCLE('',#4186,0.525);
#1630=CIRCLE('',#4188,3.);
#1631=CIRCLE('',#4189,0.525);
#1632=CIRCLE('',#4191,0.525);
#1633=CIRCLE('',#4193,0.525);
#1634=CIRCLE('',#4194,0.525);
#1635=CIRCLE('',#4196,3.);
#1636=CIRCLE('',#4198,3.);
#1637=CIRCLE('',#4199,3.);
#1638=CIRCLE('',#4200,3.);
#1639=CIRCLE('',#4201,3.);
#1640=CIRCLE('',#4202,3.);
#1641=CIRCLE('',#4203,3.);
#1642=CIRCLE('',#4204,3.);
#1643=CIRCLE('',#4205,3.);
#1644=CIRCLE('',#4207,0.275);
#1645=CIRCLE('',#4208,0.275);
#1646=CIRCLE('',#4210,0.275);
#1647=CIRCLE('',#4211,0.275);
#1648=CIRCLE('',#4213,0.275);
#1649=CIRCLE('',#4214,0.275);
#1650=CIRCLE('',#4216,0.275);
#1651=CIRCLE('',#4217,0.275);
#1652=CIRCLE('',#4219,0.275);
#1653=CIRCLE('',#4220,0.275);
#1654=CIRCLE('',#4222,0.275);
#1655=CIRCLE('',#4223,0.275);
#1656=CIRCLE('',#4225,0.34);
#1657=CIRCLE('',#4226,0.34);
#1658=CIRCLE('',#4228,2.5);
#1659=CIRCLE('',#4229,2.5);
#1660=CIRCLE('',#4233,4.);
#1661=CIRCLE('',#4234,4.);
#1662=CIRCLE('',#4238,0.1);
#1663=CIRCLE('',#4239,0.1);
#1664=CIRCLE('',#4244,0.6);
#1665=CIRCLE('',#4245,0.6);
#1666=CIRCLE('',#4248,1.2);
#1667=CIRCLE('',#4249,1.2);
#1668=CIRCLE('',#4254,0.4);
#1669=CIRCLE('',#4255,0.4);
#1670=CIRCLE('',#4260,0.165);
#1671=CIRCLE('',#4261,0.165);
#1672=CIRCLE('',#4263,0.165);
#1673=CIRCLE('',#4266,0.4);
#1674=CIRCLE('',#4267,0.4);
#1675=CIRCLE('',#4269,1.5);
#1676=CIRCLE('',#4270,1.5);
#1677=CIRCLE('',#4289,0.3);
#1678=CIRCLE('',#4291,0.35);
#1679=CIRCLE('',#4293,0.35);
#1680=CIRCLE('',#4295,0.32);
#1681=CIRCLE('',#4297,0.22);
#1682=CIRCLE('',#4299,0.1954);
#1683=CIRCLE('',#4301,0.1954);
#1684=CIRCLE('',#4303,0.16);
#1685=CIRCLE('',#4315,0.685);
#1686=CIRCLE('',#4317,0.685);
#1687=CIRCLE('',#4325,0.685);
#1688=CIRCLE('',#4327,0.605);
#1689=CIRCLE('',#4328,0.46);
#1690=CIRCLE('',#4331,0.685);
#1691=CIRCLE('',#4333,0.605);
#1692=CIRCLE('',#4335,0.46);
#1693=CIRCLE('',#4339,0.375);
#1694=CIRCLE('',#4341,0.425);
#1695=CIRCLE('',#4343,0.425);
#1696=CIRCLE('',#4345,0.395);
#1697=CIRCLE('',#4347,0.27);
#1698=CIRCLE('',#4349,0.24505);
#1699=CIRCLE('',#4351,0.24505);
#1700=CIRCLE('',#4353,0.2);
#1701=CIRCLE('',#4365,0.42);
#1702=CIRCLE('',#4366,0.42);
#1703=CIRCLE('',#4368,0.8);
#1704=CIRCLE('',#4369,0.8);
#1705=CIRCLE('',#4374,0.6175);
#1706=CIRCLE('',#4376,0.6175);
#1707=CIRCLE('',#4381,0.338975);
#1708=CIRCLE('',#4382,0.338975);
#1709=CIRCLE('',#4397,0.17);
#1710=CIRCLE('',#4399,0.1954);
#1711=CIRCLE('',#4401,0.1954);
#1712=CIRCLE('',#4403,0.125);
#1713=VERTEX_POINT('',#5623);
#1714=VERTEX_POINT('',#5625);
#1715=VERTEX_POINT('',#5629);
#1716=VERTEX_POINT('',#5631);
#1717=VERTEX_POINT('',#5635);
#1718=VERTEX_POINT('',#5636);
#1719=VERTEX_POINT('',#5638);
#1720=VERTEX_POINT('',#5640);
#1721=VERTEX_POINT('',#5644);
#1722=VERTEX_POINT('',#5646);
#1723=VERTEX_POINT('',#5650);
#1724=VERTEX_POINT('',#5652);
#1725=VERTEX_POINT('',#5662);
#1726=VERTEX_POINT('',#5664);
#1727=VERTEX_POINT('',#5668);
#1728=VERTEX_POINT('',#5669);
#1729=VERTEX_POINT('',#5671);
#1730=VERTEX_POINT('',#5673);
#1731=VERTEX_POINT('',#5677);
#1732=VERTEX_POINT('',#5679);
#1733=VERTEX_POINT('',#5683);
#1734=VERTEX_POINT('',#5685);
#1735=VERTEX_POINT('',#5695);
#1736=VERTEX_POINT('',#5697);
#1737=VERTEX_POINT('',#5701);
#1738=VERTEX_POINT('',#5702);
#1739=VERTEX_POINT('',#5704);
#1740=VERTEX_POINT('',#5706);
#1741=VERTEX_POINT('',#5710);
#1742=VERTEX_POINT('',#5712);
#1743=VERTEX_POINT('',#5716);
#1744=VERTEX_POINT('',#5718);
#1745=VERTEX_POINT('',#5728);
#1746=VERTEX_POINT('',#5730);
#1747=VERTEX_POINT('',#5735);
#1748=VERTEX_POINT('',#5737);
#1749=VERTEX_POINT('',#5742);
#1750=VERTEX_POINT('',#5744);
#1751=VERTEX_POINT('',#5749);
#1752=VERTEX_POINT('',#5751);
#1753=VERTEX_POINT('',#5756);
#1754=VERTEX_POINT('',#5758);
#1755=VERTEX_POINT('',#5763);
#1756=VERTEX_POINT('',#5765);
#1757=VERTEX_POINT('',#5770);
#1758=VERTEX_POINT('',#5771);
#1759=VERTEX_POINT('',#5813);
#1760=VERTEX_POINT('',#5815);
#1761=VERTEX_POINT('',#5823);
#1762=VERTEX_POINT('',#5825);
#1763=VERTEX_POINT('',#5863);
#1764=VERTEX_POINT('',#5865);
#1765=VERTEX_POINT('',#5867);
#1766=VERTEX_POINT('',#5886);
#1767=VERTEX_POINT('',#5910);
#1768=VERTEX_POINT('',#5914);
#1769=VERTEX_POINT('',#5915);
#1770=VERTEX_POINT('',#5926);
#1771=VERTEX_POINT('',#5955);
#1772=VERTEX_POINT('',#5960);
#1773=VERTEX_POINT('',#5962);
#1774=VERTEX_POINT('',#5967);
#1775=VERTEX_POINT('',#5969);
#1776=VERTEX_POINT('',#5974);
#1777=VERTEX_POINT('',#5980);
#1778=VERTEX_POINT('',#5982);
#1779=VERTEX_POINT('',#5987);
#1780=VERTEX_POINT('',#5990);
#1781=VERTEX_POINT('',#5995);
#1782=VERTEX_POINT('',#5998);
#1783=VERTEX_POINT('',#6005);
#1784=VERTEX_POINT('',#6007);
#1785=VERTEX_POINT('',#6010);
#1786=VERTEX_POINT('',#6015);
#1787=VERTEX_POINT('',#6021);
#1788=VERTEX_POINT('',#6023);
#1789=VERTEX_POINT('',#6027);
#1790=VERTEX_POINT('',#6029);
#1791=VERTEX_POINT('',#6036);
#1792=VERTEX_POINT('',#6038);
#1793=VERTEX_POINT('',#6041);
#1794=VERTEX_POINT('',#6045);
#1795=VERTEX_POINT('',#6047);
#1796=VERTEX_POINT('',#6050);
#1797=VERTEX_POINT('',#6052);
#1798=VERTEX_POINT('',#6057);
#1799=VERTEX_POINT('',#6064);
#1800=VERTEX_POINT('',#6066);
#1801=VERTEX_POINT('',#6743);
#1802=VERTEX_POINT('',#6745);
#1803=VERTEX_POINT('',#6812);
#1804=VERTEX_POINT('',#6814);
#1805=VERTEX_POINT('',#6818);
#1806=VERTEX_POINT('',#6820);
#1807=VERTEX_POINT('',#6827);
#1808=VERTEX_POINT('',#6829);
#1809=VERTEX_POINT('',#6833);
#1810=VERTEX_POINT('',#6835);
#1811=VERTEX_POINT('',#6839);
#1812=VERTEX_POINT('',#6841);
#1813=VERTEX_POINT('',#6845);
#1814=VERTEX_POINT('',#6847);
#1815=VERTEX_POINT('',#6851);
#1816=VERTEX_POINT('',#6853);
#1817=VERTEX_POINT('',#6857);
#1818=VERTEX_POINT('',#6859);
#1819=VERTEX_POINT('',#6863);
#1820=VERTEX_POINT('',#6865);
#1821=VERTEX_POINT('',#6869);
#1822=VERTEX_POINT('',#6871);
#1823=VERTEX_POINT('',#6878);
#1824=VERTEX_POINT('',#6880);
#1825=VERTEX_POINT('',#6884);
#1826=VERTEX_POINT('',#6886);
#1827=VERTEX_POINT('',#6891);
#1828=VERTEX_POINT('',#6894);
#1829=VERTEX_POINT('',#6896);
#1830=VERTEX_POINT('',#6900);
#1831=VERTEX_POINT('',#6907);
#1832=VERTEX_POINT('',#6908);
#1833=VERTEX_POINT('',#6912);
#1834=VERTEX_POINT('',#6914);
#1835=VERTEX_POINT('',#6918);
#1836=VERTEX_POINT('',#6919);
#1837=VERTEX_POINT('',#6921);
#1838=VERTEX_POINT('',#6923);
#1839=VERTEX_POINT('',#6929);
#1840=VERTEX_POINT('',#6930);
#1841=VERTEX_POINT('',#6934);
#1842=VERTEX_POINT('',#6936);
#1843=VERTEX_POINT('',#6940);
#1844=VERTEX_POINT('',#6941);
#1845=VERTEX_POINT('',#6945);
#1846=VERTEX_POINT('',#6947);
#1847=VERTEX_POINT('',#6951);
#1848=VERTEX_POINT('',#6952);
#1849=VERTEX_POINT('',#6956);
#1850=VERTEX_POINT('',#6958);
#1851=VERTEX_POINT('',#6962);
#1852=VERTEX_POINT('',#6963);
#1853=VERTEX_POINT('',#6965);
#1854=VERTEX_POINT('',#6967);
#1855=VERTEX_POINT('',#6973);
#1856=VERTEX_POINT('',#6975);
#1857=VERTEX_POINT('',#6985);
#1858=VERTEX_POINT('',#6987);
#1859=VERTEX_POINT('',#6991);
#1860=VERTEX_POINT('',#6993);
#1861=VERTEX_POINT('',#6997);
#1862=VERTEX_POINT('',#6999);
#1863=VERTEX_POINT('',#7003);
#1864=VERTEX_POINT('',#7005);
#1865=VERTEX_POINT('',#7009);
#1866=VERTEX_POINT('',#7011);
#1867=VERTEX_POINT('',#7015);
#1868=VERTEX_POINT('',#7017);
#1869=VERTEX_POINT('',#7021);
#1870=VERTEX_POINT('',#7023);
#1871=VERTEX_POINT('',#7027);
#1872=VERTEX_POINT('',#7029);
#1873=VERTEX_POINT('',#7035);
#1874=VERTEX_POINT('',#7037);
#1875=VERTEX_POINT('',#7753);
#1876=VERTEX_POINT('',#7755);
#1877=VERTEX_POINT('',#7832);
#1878=VERTEX_POINT('',#7834);
#1879=VERTEX_POINT('',#7839);
#1880=VERTEX_POINT('',#7841);
#1881=VERTEX_POINT('',#7848);
#1882=VERTEX_POINT('',#7850);
#1883=VERTEX_POINT('',#7857);
#1884=VERTEX_POINT('',#7858);
#1885=VERTEX_POINT('',#7860);
#1886=VERTEX_POINT('',#7864);
#1887=VERTEX_POINT('',#7875);
#1888=VERTEX_POINT('',#7887);
#1889=VERTEX_POINT('',#7926);
#1890=VERTEX_POINT('',#7928);
#1891=VERTEX_POINT('',#7932);
#1892=VERTEX_POINT('',#7934);
#1893=VERTEX_POINT('',#7941);
#1894=VERTEX_POINT('',#7942);
#1895=VERTEX_POINT('',#7944);
#1896=VERTEX_POINT('',#7946);
#1897=VERTEX_POINT('',#7950);
#1898=VERTEX_POINT('',#7952);
#1899=VERTEX_POINT('',#7956);
#1900=VERTEX_POINT('',#7958);
#1901=VERTEX_POINT('',#7968);
#1902=VERTEX_POINT('',#7969);
#1903=VERTEX_POINT('',#7971);
#1904=VERTEX_POINT('',#7973);
#1905=VERTEX_POINT('',#7977);
#1906=VERTEX_POINT('',#7979);
#1907=VERTEX_POINT('',#7983);
#1908=VERTEX_POINT('',#7985);
#1909=VERTEX_POINT('',#7995);
#1910=VERTEX_POINT('',#7998);
#1911=VERTEX_POINT('',#8002);
#1912=VERTEX_POINT('',#8006);
#1913=VERTEX_POINT('',#8010);
#1914=VERTEX_POINT('',#8013);
#1915=VERTEX_POINT('',#8017);
#1916=VERTEX_POINT('',#8021);
#1917=VERTEX_POINT('',#8026);
#1918=VERTEX_POINT('',#8027);
#1919=VERTEX_POINT('',#8029);
#1920=VERTEX_POINT('',#8031);
#1921=VERTEX_POINT('',#8035);
#1922=VERTEX_POINT('',#8037);
#1923=VERTEX_POINT('',#8041);
#1924=VERTEX_POINT('',#8043);
#1925=VERTEX_POINT('',#8047);
#1926=VERTEX_POINT('',#8049);
#1927=VERTEX_POINT('',#8053);
#1928=VERTEX_POINT('',#8055);
#1929=VERTEX_POINT('',#8065);
#1930=VERTEX_POINT('',#8066);
#1931=VERTEX_POINT('',#8068);
#1932=VERTEX_POINT('',#8070);
#1933=VERTEX_POINT('',#8072);
#1934=VERTEX_POINT('',#8074);
#1935=VERTEX_POINT('',#8077);
#1936=VERTEX_POINT('',#8080);
#1937=VERTEX_POINT('',#8081);
#1938=VERTEX_POINT('',#8083);
#1939=VERTEX_POINT('',#8085);
#1940=VERTEX_POINT('',#8087);
#1941=VERTEX_POINT('',#8089);
#1942=VERTEX_POINT('',#8092);
#1943=VERTEX_POINT('',#8107);
#1944=VERTEX_POINT('',#8111);
#1945=VERTEX_POINT('',#8113);
#1946=VERTEX_POINT('',#8118);
#1947=VERTEX_POINT('',#8122);
#1948=VERTEX_POINT('',#8126);
#1949=VERTEX_POINT('',#8132);
#1950=VERTEX_POINT('',#8135);
#1951=VERTEX_POINT('',#8139);
#1952=VERTEX_POINT('',#8143);
#1953=VERTEX_POINT('',#8147);
#1954=VERTEX_POINT('',#8150);
#1955=VERTEX_POINT('',#8154);
#1956=VERTEX_POINT('',#8158);
#1957=VERTEX_POINT('',#8163);
#1958=VERTEX_POINT('',#8164);
#1959=VERTEX_POINT('',#8166);
#1960=VERTEX_POINT('',#8168);
#1961=VERTEX_POINT('',#8172);
#1962=VERTEX_POINT('',#8174);
#1963=VERTEX_POINT('',#8178);
#1964=VERTEX_POINT('',#8180);
#1965=VERTEX_POINT('',#8184);
#1966=VERTEX_POINT('',#8186);
#1967=VERTEX_POINT('',#8190);
#1968=VERTEX_POINT('',#8192);
#1969=VERTEX_POINT('',#8202);
#1970=VERTEX_POINT('',#8204);
#1971=VERTEX_POINT('',#8208);
#1972=VERTEX_POINT('',#8210);
#1973=VERTEX_POINT('',#8217);
#1974=VERTEX_POINT('',#8218);
#1975=VERTEX_POINT('',#8222);
#1976=VERTEX_POINT('',#8226);
#1977=VERTEX_POINT('',#8229);
#1978=VERTEX_POINT('',#8233);
#1979=VERTEX_POINT('',#8237);
#1980=VERTEX_POINT('',#8245);
#1981=VERTEX_POINT('',#8247);
#1982=VERTEX_POINT('',#8249);
#1983=VERTEX_POINT('',#8253);
#1984=VERTEX_POINT('',#8257);
#1985=VERTEX_POINT('',#8261);
#1986=VERTEX_POINT('',#8265);
#1987=VERTEX_POINT('',#8280);
#1988=VERTEX_POINT('',#8282);
#1989=VERTEX_POINT('',#8294);
#1990=VERTEX_POINT('',#8295);
#1991=VERTEX_POINT('',#8297);
#1992=VERTEX_POINT('',#8299);
#1993=VERTEX_POINT('',#8303);
#1994=VERTEX_POINT('',#8305);
#1995=VERTEX_POINT('',#8309);
#1996=VERTEX_POINT('',#8311);
#1997=VERTEX_POINT('',#8315);
#1998=VERTEX_POINT('',#8317);
#1999=VERTEX_POINT('',#8321);
#2000=VERTEX_POINT('',#8323);
#2001=VERTEX_POINT('',#8331);
#2002=VERTEX_POINT('',#8334);
#2003=VERTEX_POINT('',#8338);
#2004=VERTEX_POINT('',#8342);
#2005=EDGE_CURVE('',#1713,#1713,#1530,.T.);
#2006=EDGE_CURVE('',#1713,#1714,#1042,.T.);
#2007=EDGE_CURVE('',#1714,#1714,#1531,.T.);
#2008=EDGE_CURVE('',#1715,#1715,#1532,.T.);
#2009=EDGE_CURVE('',#1715,#1716,#1043,.T.);
#2010=EDGE_CURVE('',#1716,#1716,#1533,.T.);
#2011=EDGE_CURVE('',#1717,#1718,#1044,.T.);
#2012=EDGE_CURVE('',#1718,#1719,#1045,.T.);
#2013=EDGE_CURVE('',#1720,#1719,#1046,.T.);
#2014=EDGE_CURVE('',#1717,#1720,#1047,.T.);
#2015=EDGE_CURVE('',#1721,#1717,#1048,.T.);
#2016=EDGE_CURVE('',#1722,#1720,#1049,.T.);
#2017=EDGE_CURVE('',#1721,#1722,#1050,.T.);
#2018=EDGE_CURVE('',#1723,#1721,#1051,.T.);
#2019=EDGE_CURVE('',#1724,#1722,#1052,.T.);
#2020=EDGE_CURVE('',#1723,#1724,#1053,.T.);
#2021=EDGE_CURVE('',#1718,#1723,#1054,.T.);
#2022=EDGE_CURVE('',#1719,#1724,#1055,.T.);
#2023=EDGE_CURVE('',#1725,#1725,#1534,.T.);
#2024=EDGE_CURVE('',#1725,#1726,#1056,.T.);
#2025=EDGE_CURVE('',#1726,#1726,#1535,.T.);
#2026=EDGE_CURVE('',#1727,#1728,#1057,.T.);
#2027=EDGE_CURVE('',#1728,#1729,#1058,.T.);
#2028=EDGE_CURVE('',#1730,#1729,#1059,.T.);
#2029=EDGE_CURVE('',#1727,#1730,#1060,.T.);
#2030=EDGE_CURVE('',#1731,#1727,#1061,.T.);
#2031=EDGE_CURVE('',#1732,#1730,#1062,.T.);
#2032=EDGE_CURVE('',#1731,#1732,#1063,.T.);
#2033=EDGE_CURVE('',#1733,#1731,#1064,.T.);
#2034=EDGE_CURVE('',#1734,#1732,#1065,.T.);
#2035=EDGE_CURVE('',#1733,#1734,#1066,.T.);
#2036=EDGE_CURVE('',#1728,#1733,#1067,.T.);
#2037=EDGE_CURVE('',#1729,#1734,#1068,.T.);
#2038=EDGE_CURVE('',#1735,#1735,#1536,.T.);
#2039=EDGE_CURVE('',#1735,#1736,#1069,.T.);
#2040=EDGE_CURVE('',#1736,#1736,#1537,.T.);
#2041=EDGE_CURVE('',#1737,#1738,#1070,.T.);
#2042=EDGE_CURVE('',#1738,#1739,#1071,.T.);
#2043=EDGE_CURVE('',#1740,#1739,#1072,.T.);
#2044=EDGE_CURVE('',#1737,#1740,#1073,.T.);
#2045=EDGE_CURVE('',#1741,#1737,#1074,.T.);
#2046=EDGE_CURVE('',#1742,#1740,#1075,.T.);
#2047=EDGE_CURVE('',#1741,#1742,#1076,.T.);
#2048=EDGE_CURVE('',#1743,#1741,#1077,.T.);
#2049=EDGE_CURVE('',#1744,#1742,#1078,.T.);
#2050=EDGE_CURVE('',#1743,#1744,#1079,.T.);
#2051=EDGE_CURVE('',#1738,#1743,#1080,.T.);
#2052=EDGE_CURVE('',#1739,#1744,#1081,.T.);
#2053=EDGE_CURVE('',#1745,#1745,#1538,.T.);
#2054=EDGE_CURVE('',#1745,#1746,#1082,.T.);
#2055=EDGE_CURVE('',#1746,#1746,#1539,.T.);
#2056=EDGE_CURVE('',#1747,#1747,#1540,.T.);
#2057=EDGE_CURVE('',#1747,#1748,#1083,.T.);
#2058=EDGE_CURVE('',#1748,#1748,#1541,.T.);
#2059=EDGE_CURVE('',#1749,#1749,#1542,.T.);
#2060=EDGE_CURVE('',#1749,#1750,#1084,.T.);
#2061=EDGE_CURVE('',#1750,#1750,#1543,.T.);
#2062=EDGE_CURVE('',#1751,#1751,#1544,.T.);
#2063=EDGE_CURVE('',#1751,#1752,#1085,.T.);
#2064=EDGE_CURVE('',#1752,#1752,#1545,.T.);
#2065=EDGE_CURVE('',#1753,#1753,#1546,.T.);
#2066=EDGE_CURVE('',#1753,#1754,#1086,.T.);
#2067=EDGE_CURVE('',#1754,#1754,#1547,.T.);
#2068=EDGE_CURVE('',#1755,#1755,#1548,.T.);
#2069=EDGE_CURVE('',#1755,#1756,#1087,.T.);
#2070=EDGE_CURVE('',#1756,#1756,#1549,.T.);
#2071=EDGE_CURVE('',#1757,#1758,#1550,.T.);
#2072=EDGE_CURVE('',#1758,#1757,#167,.T.);
#2073=EDGE_CURVE('',#1758,#1757,#1551,.T.);
#2074=EDGE_CURVE('',#1757,#1758,#168,.T.);
#2075=EDGE_CURVE('',#1759,#1758,#1088,.T.);
#2076=EDGE_CURVE('',#1759,#1760,#1552,.T.);
#2077=EDGE_CURVE('',#1757,#1760,#1089,.T.);
#2078=EDGE_CURVE('',#1757,#1760,#1090,.T.);
#2079=EDGE_CURVE('',#1760,#1759,#1553,.T.);
#2080=EDGE_CURVE('',#1759,#1758,#1091,.T.);
#2081=EDGE_CURVE('',#1759,#1761,#1092,.T.);
#2082=EDGE_CURVE('',#1762,#1761,#169,.T.);
#2083=EDGE_CURVE('',#1761,#1762,#170,.T.);
#2084=EDGE_CURVE('',#1763,#1763,#1554,.T.);
#2085=EDGE_CURVE('',#1763,#1764,#1093,.T.);
#2086=EDGE_CURVE('',#1765,#1764,#171,.T.);
#2087=EDGE_CURVE('',#1766,#1765,#1094,.T.);
#2088=EDGE_CURVE('',#1766,#1765,#1095,.T.);
#2089=EDGE_CURVE('',#1764,#1765,#172,.T.);
#2090=EDGE_CURVE('',#1765,#1765,#1555,.T.);
#2091=EDGE_CURVE('',#1764,#1767,#1096,.T.);
#2092=EDGE_CURVE('',#1767,#1767,#1556,.T.);
#2093=EDGE_CURVE('',#1768,#1769,#173,.T.);
#2094=EDGE_CURVE('',#1770,#1768,#174,.T.);
#2095=EDGE_CURVE('',#1769,#1770,#175,.T.);
#2096=EDGE_CURVE('',#1769,#1771,#1097,.T.);
#2097=EDGE_CURVE('',#1771,#1771,#1557,.T.);
#2098=EDGE_CURVE('',#1772,#1772,#1558,.T.);
#2099=EDGE_CURVE('',#1772,#1773,#1098,.T.);
#2100=EDGE_CURVE('',#1773,#1773,#1559,.T.);
#2101=EDGE_CURVE('',#1774,#1774,#1560,.T.);
#2102=EDGE_CURVE('',#1774,#1775,#1099,.T.);
#2103=EDGE_CURVE('',#1775,#1775,#1561,.T.);
#2104=EDGE_CURVE('',#1776,#1776,#1562,.T.);
#2105=EDGE_CURVE('',#1776,#1766,#1100,.T.);
#2106=EDGE_CURVE('',#1766,#1766,#1563,.T.);
#2107=EDGE_CURVE('',#1777,#1777,#1564,.T.);
#2108=EDGE_CURVE('',#1777,#1778,#1101,.T.);
#2109=EDGE_CURVE('',#1778,#1778,#1565,.T.);
#2110=EDGE_CURVE('',#1779,#1779,#1566,.T.);
#2111=EDGE_CURVE('',#1779,#1760,#1102,.T.);
#2112=EDGE_CURVE('',#1759,#1780,#1103,.T.);
#2113=EDGE_CURVE('',#1780,#1780,#1567,.T.);
#2114=EDGE_CURVE('',#1781,#1781,#1568,.T.);
#2115=EDGE_CURVE('',#1781,#1769,#1104,.T.);
#2116=EDGE_CURVE('',#1770,#1782,#1105,.T.);
#2117=EDGE_CURVE('',#1782,#1782,#1569,.T.);
#2118=EDGE_CURVE('',#1783,#1783,#1570,.T.);
#2119=EDGE_CURVE('',#1784,#1784,#1571,.T.);
#2120=EDGE_CURVE('',#1783,#1785,#1106,.T.);
#2121=EDGE_CURVE('',#1785,#1785,#1572,.T.);
#2122=EDGE_CURVE('',#1786,#1786,#1573,.T.);
#2123=EDGE_CURVE('',#1786,#1784,#1107,.T.);
#2124=EDGE_CURVE('',#1787,#1787,#1574,.T.);
#2125=EDGE_CURVE('',#1787,#1788,#1108,.T.);
#2126=EDGE_CURVE('',#1788,#1788,#1575,.T.);
#2127=EDGE_CURVE('',#1789,#1789,#1576,.T.);
#2128=EDGE_CURVE('',#1789,#1790,#1109,.T.);
#2129=EDGE_CURVE('',#1790,#1790,#1577,.T.);
#2130=EDGE_CURVE('',#1791,#1791,#1578,.T.);
#2131=EDGE_CURVE('',#1792,#1792,#1579,.T.);
#2132=EDGE_CURVE('',#1793,#1793,#1580,.T.);
#2133=EDGE_CURVE('',#1793,#1791,#1110,.T.);
#2134=EDGE_CURVE('',#1794,#1794,#1581,.T.);
#2135=EDGE_CURVE('',#1795,#1795,#1582,.T.);
#2136=EDGE_CURVE('',#1796,#1796,#1583,.T.);
#2137=EDGE_CURVE('',#1797,#1797,#1584,.T.);
#2138=EDGE_CURVE('',#1794,#1796,#1111,.T.);
#2139=EDGE_CURVE('',#1797,#1798,#1112,.T.);
#2140=EDGE_CURVE('',#1798,#1798,#1585,.T.);
#2141=EDGE_CURVE('',#1792,#1795,#1113,.T.);
#2142=EDGE_CURVE('',#1799,#1799,#1586,.T.);
#2143=EDGE_CURVE('',#1799,#1800,#1114,.T.);
#2144=EDGE_CURVE('',#1800,#1800,#1587,.T.);
#2145=EDGE_CURVE('',#1801,#1801,#1588,.T.);
#2146=EDGE_CURVE('',#1801,#1802,#176,.T.);
#2147=EDGE_CURVE('',#1802,#1802,#1589,.T.);
#2148=EDGE_CURVE('',#1803,#1803,#1590,.T.);
#2149=EDGE_CURVE('',#1803,#1804,#1115,.T.);
#2150=EDGE_CURVE('',#1804,#1804,#1591,.T.);
#2151=EDGE_CURVE('',#1805,#1805,#1592,.T.);
#2152=EDGE_CURVE('',#1805,#1806,#1116,.T.);
#2153=EDGE_CURVE('',#1806,#1806,#1593,.T.);
#2154=EDGE_CURVE('',#1807,#1807,#1594,.T.);
#2155=EDGE_CURVE('',#1807,#1808,#1117,.T.);
#2156=EDGE_CURVE('',#1808,#1808,#1595,.T.);
#2157=EDGE_CURVE('',#1809,#1809,#1596,.T.);
#2158=EDGE_CURVE('',#1809,#1810,#1118,.T.);
#2159=EDGE_CURVE('',#1810,#1810,#1597,.T.);
#2160=EDGE_CURVE('',#1811,#1811,#1598,.T.);
#2161=EDGE_CURVE('',#1811,#1812,#1119,.T.);
#2162=EDGE_CURVE('',#1812,#1812,#1599,.T.);
#2163=EDGE_CURVE('',#1813,#1813,#1600,.T.);
#2164=EDGE_CURVE('',#1813,#1814,#1120,.T.);
#2165=EDGE_CURVE('',#1814,#1814,#1601,.T.);
#2166=EDGE_CURVE('',#1815,#1815,#1602,.T.);
#2167=EDGE_CURVE('',#1815,#1816,#1121,.T.);
#2168=EDGE_CURVE('',#1816,#1816,#1603,.T.);
#2169=EDGE_CURVE('',#1817,#1817,#1604,.T.);
#2170=EDGE_CURVE('',#1817,#1818,#1122,.T.);
#2171=EDGE_CURVE('',#1818,#1818,#1605,.T.);
#2172=EDGE_CURVE('',#1819,#1819,#1606,.T.);
#2173=EDGE_CURVE('',#1819,#1820,#1123,.T.);
#2174=EDGE_CURVE('',#1820,#1820,#1607,.T.);
#2175=EDGE_CURVE('',#1821,#1821,#1608,.T.);
#2176=EDGE_CURVE('',#1821,#1822,#1124,.T.);
#2177=EDGE_CURVE('',#1822,#1822,#1609,.T.);
#2178=EDGE_CURVE('',#1823,#1823,#1610,.T.);
#2179=EDGE_CURVE('',#1823,#1824,#1125,.T.);
#2180=EDGE_CURVE('',#1824,#1824,#1611,.T.);
#2181=EDGE_CURVE('',#1825,#1825,#1612,.T.);
#2182=EDGE_CURVE('',#1825,#1826,#1126,.T.);
#2183=EDGE_CURVE('',#1826,#1826,#1613,.T.);
#2184=EDGE_CURVE('',#1827,#1827,#1614,.T.);
#2185=EDGE_CURVE('',#1828,#1828,#1615,.T.);
#2186=EDGE_CURVE('',#1828,#1829,#1127,.T.);
#2187=EDGE_CURVE('',#1829,#1829,#1616,.T.);
#2188=EDGE_CURVE('',#1827,#1830,#1128,.T.);
#2189=EDGE_CURVE('',#1830,#1830,#1617,.T.);
#2190=EDGE_CURVE('',#1831,#1832,#1618,.T.);
#2191=EDGE_CURVE('',#1832,#1831,#1619,.T.);
#2192=EDGE_CURVE('',#1833,#1831,#1129,.T.);
#2193=EDGE_CURVE('',#1834,#1833,#1620,.T.);
#2194=EDGE_CURVE('',#1832,#1834,#1130,.T.);
#2195=EDGE_CURVE('',#1835,#1836,#1131,.T.);
#2196=EDGE_CURVE('',#1835,#1837,#1621,.T.);
#2197=EDGE_CURVE('',#1838,#1837,#1132,.T.);
#2198=EDGE_CURVE('',#1836,#1838,#1622,.T.);
#2199=EDGE_CURVE('',#1837,#1835,#1623,.T.);
#2200=EDGE_CURVE('',#1839,#1840,#1624,.T.);
#2201=EDGE_CURVE('',#1840,#1839,#1625,.T.);
#2202=EDGE_CURVE('',#1841,#1839,#1133,.T.);
#2203=EDGE_CURVE('',#1842,#1841,#1626,.T.);
#2204=EDGE_CURVE('',#1840,#1842,#1134,.T.);
#2205=EDGE_CURVE('',#1843,#1844,#1627,.T.);
#2206=EDGE_CURVE('',#1844,#1843,#1628,.T.);
#2207=EDGE_CURVE('',#1845,#1843,#1135,.T.);
#2208=EDGE_CURVE('',#1846,#1845,#1629,.T.);
#2209=EDGE_CURVE('',#1844,#1846,#1136,.T.);
#2210=EDGE_CURVE('',#1847,#1848,#1630,.T.);
#2211=EDGE_CURVE('',#1848,#1847,#1631,.T.);
#2212=EDGE_CURVE('',#1849,#1847,#1137,.T.);
#2213=EDGE_CURVE('',#1850,#1849,#1632,.T.);
#2214=EDGE_CURVE('',#1848,#1850,#1138,.T.);
#2215=EDGE_CURVE('',#1851,#1852,#1139,.T.);
#2216=EDGE_CURVE('',#1851,#1853,#1633,.T.);
#2217=EDGE_CURVE('',#1854,#1853,#1140,.T.);
#2218=EDGE_CURVE('',#1852,#1854,#1634,.T.);
#2219=EDGE_CURVE('',#1853,#1851,#1635,.T.);
#2220=EDGE_CURVE('',#1855,#1855,#1636,.T.);
#2221=EDGE_CURVE('',#1855,#1856,#1141,.T.);
#2222=EDGE_CURVE('',#1849,#1856,#1637,.T.);
#2223=EDGE_CURVE('',#1833,#1850,#1638,.T.);
#2224=EDGE_CURVE('',#1854,#1834,#1639,.T.);
#2225=EDGE_CURVE('',#1838,#1852,#1640,.T.);
#2226=EDGE_CURVE('',#1841,#1836,#1641,.T.);
#2227=EDGE_CURVE('',#1845,#1842,#1642,.T.);
#2228=EDGE_CURVE('',#1856,#1846,#1643,.T.);
#2229=EDGE_CURVE('',#1857,#1857,#1644,.T.);
#2230=EDGE_CURVE('',#1857,#1858,#1142,.T.);
#2231=EDGE_CURVE('',#1858,#1858,#1645,.T.);
#2232=EDGE_CURVE('',#1859,#1859,#1646,.T.);
#2233=EDGE_CURVE('',#1859,#1860,#1143,.T.);
#2234=EDGE_CURVE('',#1860,#1860,#1647,.T.);
#2235=EDGE_CURVE('',#1861,#1861,#1648,.T.);
#2236=EDGE_CURVE('',#1861,#1862,#1144,.T.);
#2237=EDGE_CURVE('',#1862,#1862,#1649,.T.);
#2238=EDGE_CURVE('',#1863,#1863,#1650,.T.);
#2239=EDGE_CURVE('',#1863,#1864,#1145,.T.);
#2240=EDGE_CURVE('',#1864,#1864,#1651,.T.);
#2241=EDGE_CURVE('',#1865,#1865,#1652,.T.);
#2242=EDGE_CURVE('',#1865,#1866,#1146,.T.);
#2243=EDGE_CURVE('',#1866,#1866,#1653,.T.);
#2244=EDGE_CURVE('',#1867,#1867,#1654,.T.);
#2245=EDGE_CURVE('',#1867,#1868,#1147,.T.);
#2246=EDGE_CURVE('',#1868,#1868,#1655,.T.);
#2247=EDGE_CURVE('',#1869,#1869,#1656,.T.);
#2248=EDGE_CURVE('',#1869,#1870,#1148,.T.);
#2249=EDGE_CURVE('',#1870,#1870,#1657,.T.);
#2250=EDGE_CURVE('',#1871,#1871,#1658,.T.);
#2251=EDGE_CURVE('',#1871,#1872,#1149,.T.);
#2252=EDGE_CURVE('',#1872,#1872,#1659,.T.);
#2253=EDGE_CURVE('',#1873,#1873,#1660,.T.);
#2254=EDGE_CURVE('',#1873,#1874,#1150,.T.);
#2255=EDGE_CURVE('',#1874,#1874,#1661,.T.);
#2256=EDGE_CURVE('',#1875,#1875,#1662,.T.);
#2257=EDGE_CURVE('',#1875,#1876,#177,.T.);
#2258=EDGE_CURVE('',#1876,#1876,#1663,.T.);
#2259=EDGE_CURVE('',#1877,#1877,#1664,.T.);
#2260=EDGE_CURVE('',#1877,#1878,#1151,.T.);
#2261=EDGE_CURVE('',#1878,#1878,#1665,.T.);
#2262=EDGE_CURVE('',#1879,#1879,#1666,.T.);
#2263=EDGE_CURVE('',#1879,#1880,#1152,.T.);
#2264=EDGE_CURVE('',#1880,#1880,#1667,.T.);
#2265=EDGE_CURVE('',#1881,#1881,#1668,.T.);
#2266=EDGE_CURVE('',#1881,#1882,#1153,.T.);
#2267=EDGE_CURVE('',#1882,#1882,#1669,.T.);
#2268=EDGE_CURVE('',#1883,#1884,#1154,.T.);
#2269=EDGE_CURVE('',#1883,#1885,#1670,.T.);
#2270=EDGE_CURVE('',#1885,#1884,#1671,.T.);
#2271=EDGE_CURVE('',#1886,#1883,#178,.T.);
#2272=EDGE_CURVE('',#1887,#1886,#1672,.T.);
#2273=EDGE_CURVE('',#1884,#1887,#179,.T.);
#2274=EDGE_CURVE('',#1885,#1888,#1155,.T.);
#2275=EDGE_CURVE('',#1888,#1888,#180,.T.);
#2276=EDGE_CURVE('',#1887,#1886,#1156,.T.);
#2277=EDGE_CURVE('',#1889,#1889,#1673,.T.);
#2278=EDGE_CURVE('',#1889,#1890,#1157,.T.);
#2279=EDGE_CURVE('',#1890,#1890,#1674,.T.);
#2280=EDGE_CURVE('',#1891,#1891,#1675,.T.);
#2281=EDGE_CURVE('',#1891,#1892,#1158,.T.);
#2282=EDGE_CURVE('',#1892,#1892,#1676,.T.);
#2283=EDGE_CURVE('',#1893,#1894,#1159,.T.);
#2284=EDGE_CURVE('',#1894,#1895,#1160,.T.);
#2285=EDGE_CURVE('',#1896,#1895,#1161,.T.);
#2286=EDGE_CURVE('',#1893,#1896,#1162,.T.);
#2287=EDGE_CURVE('',#1897,#1893,#1163,.T.);
#2288=EDGE_CURVE('',#1898,#1896,#1164,.T.);
#2289=EDGE_CURVE('',#1897,#1898,#1165,.T.);
#2290=EDGE_CURVE('',#1899,#1897,#1166,.T.);
#2291=EDGE_CURVE('',#1900,#1898,#1167,.T.);
#2292=EDGE_CURVE('',#1899,#1900,#1168,.T.);
#2293=EDGE_CURVE('',#1894,#1899,#1169,.T.);
#2294=EDGE_CURVE('',#1895,#1900,#1170,.T.);
#2295=EDGE_CURVE('',#1901,#1902,#1171,.T.);
#2296=EDGE_CURVE('',#1902,#1903,#1172,.T.);
#2297=EDGE_CURVE('',#1904,#1903,#1173,.T.);
#2298=EDGE_CURVE('',#1901,#1904,#1174,.T.);
#2299=EDGE_CURVE('',#1905,#1901,#1175,.T.);
#2300=EDGE_CURVE('',#1906,#1904,#1176,.T.);
#2301=EDGE_CURVE('',#1905,#1906,#1177,.T.);
#2302=EDGE_CURVE('',#1907,#1905,#1178,.T.);
#2303=EDGE_CURVE('',#1908,#1906,#1179,.T.);
#2304=EDGE_CURVE('',#1907,#1908,#1180,.T.);
#2305=EDGE_CURVE('',#1902,#1907,#1181,.T.);
#2306=EDGE_CURVE('',#1903,#1908,#1182,.T.);
#2307=EDGE_CURVE('',#1909,#1909,#1677,.T.);
#2308=EDGE_CURVE('',#1910,#1910,#1678,.T.);
#2309=EDGE_CURVE('',#1910,#1909,#1183,.T.);
#2310=EDGE_CURVE('',#1911,#1911,#1679,.T.);
#2311=EDGE_CURVE('',#1911,#1910,#1184,.T.);
#2312=EDGE_CURVE('',#1912,#1912,#1680,.T.);
#2313=EDGE_CURVE('',#1912,#1911,#1185,.T.);
#2314=EDGE_CURVE('',#1913,#1913,#1681,.T.);
#2315=EDGE_CURVE('',#1914,#1914,#1682,.F.);
#2316=EDGE_CURVE('',#1914,#1913,#1186,.T.);
#2317=EDGE_CURVE('',#1915,#1915,#1683,.F.);
#2318=EDGE_CURVE('',#1915,#1914,#1187,.T.);
#2319=EDGE_CURVE('',#1916,#1916,#1684,.T.);
#2320=EDGE_CURVE('',#1916,#1915,#1188,.T.);
#2321=EDGE_CURVE('',#1917,#1918,#1189,.T.);
#2322=EDGE_CURVE('',#1918,#1919,#1190,.T.);
#2323=EDGE_CURVE('',#1919,#1920,#1191,.T.);
#2324=EDGE_CURVE('',#1917,#1920,#1192,.T.);
#2325=EDGE_CURVE('',#1918,#1921,#1193,.T.);
#2326=EDGE_CURVE('',#1921,#1922,#1194,.T.);
#2327=EDGE_CURVE('',#1922,#1919,#1195,.T.);
#2328=EDGE_CURVE('',#1921,#1923,#1196,.T.);
#2329=EDGE_CURVE('',#1923,#1924,#1197,.T.);
#2330=EDGE_CURVE('',#1924,#1922,#1198,.T.);
#2331=EDGE_CURVE('',#1923,#1925,#1199,.T.);
#2332=EDGE_CURVE('',#1925,#1926,#1200,.T.);
#2333=EDGE_CURVE('',#1926,#1924,#1201,.T.);
#2334=EDGE_CURVE('',#1925,#1927,#1202,.T.);
#2335=EDGE_CURVE('',#1927,#1928,#1203,.T.);
#2336=EDGE_CURVE('',#1928,#1926,#1204,.T.);
#2337=EDGE_CURVE('',#1927,#1917,#1205,.T.);
#2338=EDGE_CURVE('',#1920,#1928,#1206,.T.);
#2339=EDGE_CURVE('',#1929,#1930,#1207,.T.);
#2340=EDGE_CURVE('',#1930,#1931,#1208,.T.);
#2341=EDGE_CURVE('',#1931,#1932,#1209,.T.);
#2342=EDGE_CURVE('',#1932,#1933,#1210,.T.);
#2343=EDGE_CURVE('',#1933,#1934,#1211,.T.);
#2344=EDGE_CURVE('',#1934,#1929,#1212,.T.);
#2345=EDGE_CURVE('',#1935,#1935,#1685,.T.);
#2346=EDGE_CURVE('',#1936,#1937,#1213,.T.);
#2347=EDGE_CURVE('',#1937,#1938,#1214,.T.);
#2348=EDGE_CURVE('',#1938,#1939,#1215,.T.);
#2349=EDGE_CURVE('',#1939,#1940,#1216,.T.);
#2350=EDGE_CURVE('',#1940,#1941,#1217,.T.);
#2351=EDGE_CURVE('',#1941,#1936,#1218,.T.);
#2352=EDGE_CURVE('',#1942,#1942,#1686,.T.);
#2353=EDGE_CURVE('',#1936,#1930,#1219,.T.);
#2354=EDGE_CURVE('',#1931,#1941,#1220,.T.);
#2355=EDGE_CURVE('',#1932,#1940,#1221,.T.);
#2356=EDGE_CURVE('',#1933,#1939,#1222,.T.);
#2357=EDGE_CURVE('',#1934,#1938,#1223,.T.);
#2358=EDGE_CURVE('',#1929,#1937,#1224,.T.);
#2359=EDGE_CURVE('',#1942,#1943,#1225,.T.);
#2360=EDGE_CURVE('',#1943,#1943,#1687,.T.);
#2361=EDGE_CURVE('',#1944,#1944,#1688,.T.);
#2362=EDGE_CURVE('',#1945,#1945,#1689,.T.);
#2363=EDGE_CURVE('',#1943,#1944,#1226,.T.);
#2364=EDGE_CURVE('',#1946,#1946,#1690,.T.);
#2365=EDGE_CURVE('',#1946,#1935,#1227,.T.);
#2366=EDGE_CURVE('',#1947,#1947,#1691,.T.);
#2367=EDGE_CURVE('',#1947,#1946,#1228,.T.);
#2368=EDGE_CURVE('',#1948,#1948,#1692,.T.);
#2369=EDGE_CURVE('',#1948,#1945,#1229,.T.);
#2370=EDGE_CURVE('',#1949,#1949,#1693,.T.);
#2371=EDGE_CURVE('',#1950,#1950,#1694,.T.);
#2372=EDGE_CURVE('',#1950,#1949,#1230,.T.);
#2373=EDGE_CURVE('',#1951,#1951,#1695,.T.);
#2374=EDGE_CURVE('',#1951,#1950,#1231,.T.);
#2375=EDGE_CURVE('',#1952,#1952,#1696,.T.);
#2376=EDGE_CURVE('',#1952,#1951,#1232,.T.);
#2377=EDGE_CURVE('',#1953,#1953,#1697,.T.);
#2378=EDGE_CURVE('',#1954,#1954,#1698,.F.);
#2379=EDGE_CURVE('',#1954,#1953,#1233,.T.);
#2380=EDGE_CURVE('',#1955,#1955,#1699,.F.);
#2381=EDGE_CURVE('',#1955,#1954,#1234,.T.);
#2382=EDGE_CURVE('',#1956,#1956,#1700,.T.);
#2383=EDGE_CURVE('',#1956,#1955,#1235,.T.);
#2384=EDGE_CURVE('',#1957,#1958,#1236,.T.);
#2385=EDGE_CURVE('',#1958,#1959,#1237,.T.);
#2386=EDGE_CURVE('',#1959,#1960,#1238,.T.);
#2387=EDGE_CURVE('',#1957,#1960,#1239,.T.);
#2388=EDGE_CURVE('',#1958,#1961,#1240,.T.);
#2389=EDGE_CURVE('',#1961,#1962,#1241,.T.);
#2390=EDGE_CURVE('',#1962,#1959,#1242,.T.);
#2391=EDGE_CURVE('',#1961,#1963,#1243,.T.);
#2392=EDGE_CURVE('',#1963,#1964,#1244,.T.);
#2393=EDGE_CURVE('',#1964,#1962,#1245,.T.);
#2394=EDGE_CURVE('',#1963,#1965,#1246,.T.);
#2395=EDGE_CURVE('',#1965,#1966,#1247,.T.);
#2396=EDGE_CURVE('',#1966,#1964,#1248,.T.);
#2397=EDGE_CURVE('',#1965,#1967,#1249,.T.);
#2398=EDGE_CURVE('',#1967,#1968,#1250,.T.);
#2399=EDGE_CURVE('',#1968,#1966,#1251,.T.);
#2400=EDGE_CURVE('',#1967,#1957,#1252,.T.);
#2401=EDGE_CURVE('',#1960,#1968,#1253,.T.);
#2402=EDGE_CURVE('',#1969,#1969,#1701,.T.);
#2403=EDGE_CURVE('',#1969,#1970,#1254,.T.);
#2404=EDGE_CURVE('',#1970,#1970,#1702,.T.);
#2405=EDGE_CURVE('',#1971,#1971,#1703,.T.);
#2406=EDGE_CURVE('',#1971,#1972,#1255,.T.);
#2407=EDGE_CURVE('',#1972,#1972,#1704,.T.);
#2408=EDGE_CURVE('',#1973,#1974,#135,.T.);
#2409=EDGE_CURVE('',#1975,#1973,#136,.T.);
#2410=EDGE_CURVE('',#1975,#1976,#1256,.T.);
#2411=EDGE_CURVE('',#1976,#1976,#1705,.T.);
#2412=EDGE_CURVE('',#1977,#1975,#137,.T.);
#2413=EDGE_CURVE('',#1978,#1977,#138,.T.);
#2414=EDGE_CURVE('',#1979,#1978,#139,.T.);
#2415=EDGE_CURVE('',#1974,#1979,#140,.T.);
#2416=EDGE_CURVE('',#1980,#1980,#1706,.T.);
#2417=EDGE_CURVE('',#1980,#1981,#1257,.T.);
#2418=EDGE_CURVE('',#1982,#1981,#141,.T.);
#2419=EDGE_CURVE('',#1983,#1982,#142,.T.);
#2420=EDGE_CURVE('',#1984,#1983,#143,.T.);
#2421=EDGE_CURVE('',#1985,#1984,#144,.T.);
#2422=EDGE_CURVE('',#1986,#1985,#145,.T.);
#2423=EDGE_CURVE('',#1981,#1986,#146,.T.);
#2424=EDGE_CURVE('',#1977,#1986,#1258,.T.);
#2425=EDGE_CURVE('',#1978,#1985,#1259,.T.);
#2426=EDGE_CURVE('',#1975,#1981,#1260,.T.);
#2427=EDGE_CURVE('',#1973,#1982,#1261,.T.);
#2428=EDGE_CURVE('',#1987,#1987,#1707,.F.);
#2429=EDGE_CURVE('',#1987,#1988,#1262,.T.);
#2430=EDGE_CURVE('',#1988,#1988,#1708,.F.);
#2431=EDGE_CURVE('',#1974,#1983,#1263,.T.);
#2432=EDGE_CURVE('',#1979,#1984,#1264,.T.);
#2433=EDGE_CURVE('',#1989,#1990,#1265,.T.);
#2434=EDGE_CURVE('',#1989,#1991,#1266,.T.);
#2435=EDGE_CURVE('',#1991,#1992,#1267,.T.);
#2436=EDGE_CURVE('',#1990,#1992,#1268,.T.);
#2437=EDGE_CURVE('',#1993,#1989,#1269,.T.);
#2438=EDGE_CURVE('',#1993,#1994,#1270,.T.);
#2439=EDGE_CURVE('',#1994,#1991,#1271,.T.);
#2440=EDGE_CURVE('',#1995,#1993,#1272,.T.);
#2441=EDGE_CURVE('',#1995,#1996,#1273,.T.);
#2442=EDGE_CURVE('',#1996,#1994,#1274,.T.);
#2443=EDGE_CURVE('',#1997,#1995,#1275,.T.);
#2444=EDGE_CURVE('',#1997,#1998,#1276,.T.);
#2445=EDGE_CURVE('',#1998,#1996,#1277,.T.);
#2446=EDGE_CURVE('',#1999,#1997,#1278,.T.);
#2447=EDGE_CURVE('',#1999,#2000,#1279,.T.);
#2448=EDGE_CURVE('',#2000,#1998,#1280,.T.);
#2449=EDGE_CURVE('',#1990,#1999,#1281,.T.);
#2450=EDGE_CURVE('',#1992,#2000,#1282,.T.);
#2451=EDGE_CURVE('',#2001,#2001,#1709,.T.);
#2452=EDGE_CURVE('',#2002,#2002,#1710,.T.);
#2453=EDGE_CURVE('',#2002,#2001,#1283,.T.);
#2454=EDGE_CURVE('',#2003,#2003,#1711,.F.);
#2455=EDGE_CURVE('',#2003,#2002,#1284,.T.);
#2456=EDGE_CURVE('',#2004,#2004,#1712,.T.);
#2457=EDGE_CURVE('',#2004,#2003,#1285,.T.);
#2458=ORIENTED_EDGE('',*,*,#2005,.F.);
#2459=ORIENTED_EDGE('',*,*,#2006,.T.);
#2460=ORIENTED_EDGE('',*,*,#2007,.F.);
#2461=ORIENTED_EDGE('',*,*,#2006,.F.);
#2462=ORIENTED_EDGE('',*,*,#2008,.F.);
#2463=ORIENTED_EDGE('',*,*,#2009,.T.);
#2464=ORIENTED_EDGE('',*,*,#2010,.F.);
#2465=ORIENTED_EDGE('',*,*,#2009,.F.);
#2466=ORIENTED_EDGE('',*,*,#2011,.T.);
#2467=ORIENTED_EDGE('',*,*,#2012,.T.);
#2468=ORIENTED_EDGE('',*,*,#2013,.F.);
#2469=ORIENTED_EDGE('',*,*,#2014,.F.);
#2470=ORIENTED_EDGE('',*,*,#2015,.T.);
#2471=ORIENTED_EDGE('',*,*,#2014,.T.);
#2472=ORIENTED_EDGE('',*,*,#2016,.F.);
#2473=ORIENTED_EDGE('',*,*,#2017,.F.);
#2474=ORIENTED_EDGE('',*,*,#2018,.T.);
#2475=ORIENTED_EDGE('',*,*,#2017,.T.);
#2476=ORIENTED_EDGE('',*,*,#2019,.F.);
#2477=ORIENTED_EDGE('',*,*,#2020,.F.);
#2478=ORIENTED_EDGE('',*,*,#2021,.T.);
#2479=ORIENTED_EDGE('',*,*,#2020,.T.);
#2480=ORIENTED_EDGE('',*,*,#2022,.F.);
#2481=ORIENTED_EDGE('',*,*,#2012,.F.);
#2482=ORIENTED_EDGE('',*,*,#2022,.T.);
#2483=ORIENTED_EDGE('',*,*,#2019,.T.);
#2484=ORIENTED_EDGE('',*,*,#2016,.T.);
#2485=ORIENTED_EDGE('',*,*,#2013,.T.);
#2486=ORIENTED_EDGE('',*,*,#2007,.T.);
#2487=ORIENTED_EDGE('',*,*,#2010,.T.);
#2488=ORIENTED_EDGE('',*,*,#2021,.F.);
#2489=ORIENTED_EDGE('',*,*,#2011,.F.);
#2490=ORIENTED_EDGE('',*,*,#2015,.F.);
#2491=ORIENTED_EDGE('',*,*,#2018,.F.);
#2492=ORIENTED_EDGE('',*,*,#2005,.T.);
#2493=ORIENTED_EDGE('',*,*,#2008,.T.);
#2494=ORIENTED_EDGE('',*,*,#2023,.F.);
#2495=ORIENTED_EDGE('',*,*,#2024,.T.);
#2496=ORIENTED_EDGE('',*,*,#2025,.F.);
#2497=ORIENTED_EDGE('',*,*,#2024,.F.);
#2498=ORIENTED_EDGE('',*,*,#2026,.T.);
#2499=ORIENTED_EDGE('',*,*,#2027,.T.);
#2500=ORIENTED_EDGE('',*,*,#2028,.F.);
#2501=ORIENTED_EDGE('',*,*,#2029,.F.);
#2502=ORIENTED_EDGE('',*,*,#2030,.T.);
#2503=ORIENTED_EDGE('',*,*,#2029,.T.);
#2504=ORIENTED_EDGE('',*,*,#2031,.F.);
#2505=ORIENTED_EDGE('',*,*,#2032,.F.);
#2506=ORIENTED_EDGE('',*,*,#2033,.T.);
#2507=ORIENTED_EDGE('',*,*,#2032,.T.);
#2508=ORIENTED_EDGE('',*,*,#2034,.F.);
#2509=ORIENTED_EDGE('',*,*,#2035,.F.);
#2510=ORIENTED_EDGE('',*,*,#2036,.T.);
#2511=ORIENTED_EDGE('',*,*,#2035,.T.);
#2512=ORIENTED_EDGE('',*,*,#2037,.F.);
#2513=ORIENTED_EDGE('',*,*,#2027,.F.);
#2514=ORIENTED_EDGE('',*,*,#2037,.T.);
#2515=ORIENTED_EDGE('',*,*,#2034,.T.);
#2516=ORIENTED_EDGE('',*,*,#2031,.T.);
#2517=ORIENTED_EDGE('',*,*,#2028,.T.);
#2518=ORIENTED_EDGE('',*,*,#2025,.T.);
#2519=ORIENTED_EDGE('',*,*,#2036,.F.);
#2520=ORIENTED_EDGE('',*,*,#2026,.F.);
#2521=ORIENTED_EDGE('',*,*,#2030,.F.);
#2522=ORIENTED_EDGE('',*,*,#2033,.F.);
#2523=ORIENTED_EDGE('',*,*,#2023,.T.);
#2524=ORIENTED_EDGE('',*,*,#2038,.F.);
#2525=ORIENTED_EDGE('',*,*,#2039,.T.);
#2526=ORIENTED_EDGE('',*,*,#2040,.F.);
#2527=ORIENTED_EDGE('',*,*,#2039,.F.);
#2528=ORIENTED_EDGE('',*,*,#2041,.T.);
#2529=ORIENTED_EDGE('',*,*,#2042,.T.);
#2530=ORIENTED_EDGE('',*,*,#2043,.F.);
#2531=ORIENTED_EDGE('',*,*,#2044,.F.);
#2532=ORIENTED_EDGE('',*,*,#2045,.T.);
#2533=ORIENTED_EDGE('',*,*,#2044,.T.);
#2534=ORIENTED_EDGE('',*,*,#2046,.F.);
#2535=ORIENTED_EDGE('',*,*,#2047,.F.);
#2536=ORIENTED_EDGE('',*,*,#2048,.T.);
#2537=ORIENTED_EDGE('',*,*,#2047,.T.);
#2538=ORIENTED_EDGE('',*,*,#2049,.F.);
#2539=ORIENTED_EDGE('',*,*,#2050,.F.);
#2540=ORIENTED_EDGE('',*,*,#2051,.T.);
#2541=ORIENTED_EDGE('',*,*,#2050,.T.);
#2542=ORIENTED_EDGE('',*,*,#2052,.F.);
#2543=ORIENTED_EDGE('',*,*,#2042,.F.);
#2544=ORIENTED_EDGE('',*,*,#2052,.T.);
#2545=ORIENTED_EDGE('',*,*,#2049,.T.);
#2546=ORIENTED_EDGE('',*,*,#2046,.T.);
#2547=ORIENTED_EDGE('',*,*,#2043,.T.);
#2548=ORIENTED_EDGE('',*,*,#2040,.T.);
#2549=ORIENTED_EDGE('',*,*,#2051,.F.);
#2550=ORIENTED_EDGE('',*,*,#2041,.F.);
#2551=ORIENTED_EDGE('',*,*,#2045,.F.);
#2552=ORIENTED_EDGE('',*,*,#2048,.F.);
#2553=ORIENTED_EDGE('',*,*,#2038,.T.);
#2554=ORIENTED_EDGE('',*,*,#2053,.F.);
#2555=ORIENTED_EDGE('',*,*,#2054,.T.);
#2556=ORIENTED_EDGE('',*,*,#2055,.F.);
#2557=ORIENTED_EDGE('',*,*,#2054,.F.);
#2558=ORIENTED_EDGE('',*,*,#2053,.T.);
#2559=ORIENTED_EDGE('',*,*,#2056,.F.);
#2560=ORIENTED_EDGE('',*,*,#2057,.T.);
#2561=ORIENTED_EDGE('',*,*,#2058,.F.);
#2562=ORIENTED_EDGE('',*,*,#2057,.F.);
#2563=ORIENTED_EDGE('',*,*,#2056,.T.);
#2564=ORIENTED_EDGE('',*,*,#2059,.F.);
#2565=ORIENTED_EDGE('',*,*,#2060,.T.);
#2566=ORIENTED_EDGE('',*,*,#2061,.F.);
#2567=ORIENTED_EDGE('',*,*,#2060,.F.);
#2568=ORIENTED_EDGE('',*,*,#2059,.T.);
#2569=ORIENTED_EDGE('',*,*,#2062,.F.);
#2570=ORIENTED_EDGE('',*,*,#2063,.T.);
#2571=ORIENTED_EDGE('',*,*,#2064,.F.);
#2572=ORIENTED_EDGE('',*,*,#2063,.F.);
#2573=ORIENTED_EDGE('',*,*,#2062,.T.);
#2574=ORIENTED_EDGE('',*,*,#2065,.F.);
#2575=ORIENTED_EDGE('',*,*,#2066,.T.);
#2576=ORIENTED_EDGE('',*,*,#2067,.F.);
#2577=ORIENTED_EDGE('',*,*,#2066,.F.);
#2578=ORIENTED_EDGE('',*,*,#2065,.T.);
#2579=ORIENTED_EDGE('',*,*,#2068,.F.);
#2580=ORIENTED_EDGE('',*,*,#2069,.T.);
#2581=ORIENTED_EDGE('',*,*,#2070,.F.);
#2582=ORIENTED_EDGE('',*,*,#2069,.F.);
#2583=ORIENTED_EDGE('',*,*,#2068,.T.);
#2584=ORIENTED_EDGE('',*,*,#2071,.F.);
#2585=ORIENTED_EDGE('',*,*,#2072,.F.);
#2586=ORIENTED_EDGE('',*,*,#2073,.F.);
#2587=ORIENTED_EDGE('',*,*,#2074,.F.);
#2588=ORIENTED_EDGE('',*,*,#2071,.T.);
#2589=ORIENTED_EDGE('',*,*,#2075,.F.);
#2590=ORIENTED_EDGE('',*,*,#2076,.T.);
#2591=ORIENTED_EDGE('',*,*,#2077,.F.);
#2592=ORIENTED_EDGE('',*,*,#2073,.T.);
#2593=ORIENTED_EDGE('',*,*,#2078,.T.);
#2594=ORIENTED_EDGE('',*,*,#2079,.T.);
#2595=ORIENTED_EDGE('',*,*,#2080,.T.);
#2596=ORIENTED_EDGE('',*,*,#2076,.F.);
#2597=ORIENTED_EDGE('',*,*,#2081,.T.);
#2598=ORIENTED_EDGE('',*,*,#2082,.F.);
#2599=ORIENTED_EDGE('',*,*,#2083,.F.);
#2600=ORIENTED_EDGE('',*,*,#2081,.F.);
#2601=ORIENTED_EDGE('',*,*,#2079,.F.);
#2602=ORIENTED_EDGE('',*,*,#2084,.F.);
#2603=ORIENTED_EDGE('',*,*,#2085,.T.);
#2604=ORIENTED_EDGE('',*,*,#2086,.F.);
#2605=ORIENTED_EDGE('',*,*,#2087,.F.);
#2606=ORIENTED_EDGE('',*,*,#2088,.T.);
#2607=ORIENTED_EDGE('',*,*,#2089,.F.);
#2608=ORIENTED_EDGE('',*,*,#2085,.F.);
#2609=ORIENTED_EDGE('',*,*,#2090,.T.);
#2610=ORIENTED_EDGE('',*,*,#2086,.T.);
#2611=ORIENTED_EDGE('',*,*,#2091,.T.);
#2612=ORIENTED_EDGE('',*,*,#2092,.T.);
#2613=ORIENTED_EDGE('',*,*,#2091,.F.);
#2614=ORIENTED_EDGE('',*,*,#2089,.T.);
#2615=ORIENTED_EDGE('',*,*,#2093,.F.);
#2616=ORIENTED_EDGE('',*,*,#2094,.F.);
#2617=ORIENTED_EDGE('',*,*,#2095,.F.);
#2618=ORIENTED_EDGE('',*,*,#2096,.T.);
#2619=ORIENTED_EDGE('',*,*,#2097,.T.);
#2620=ORIENTED_EDGE('',*,*,#2096,.F.);
#2621=ORIENTED_EDGE('',*,*,#2097,.F.);
#2622=ORIENTED_EDGE('',*,*,#2084,.T.);
#2623=ORIENTED_EDGE('',*,*,#2098,.F.);
#2624=ORIENTED_EDGE('',*,*,#2099,.T.);
#2625=ORIENTED_EDGE('',*,*,#2100,.T.);
#2626=ORIENTED_EDGE('',*,*,#2099,.F.);
#2627=ORIENTED_EDGE('',*,*,#2100,.F.);
#2628=ORIENTED_EDGE('',*,*,#2101,.F.);
#2629=ORIENTED_EDGE('',*,*,#2102,.T.);
#2630=ORIENTED_EDGE('',*,*,#2103,.T.);
#2631=ORIENTED_EDGE('',*,*,#2102,.F.);
#2632=ORIENTED_EDGE('',*,*,#2103,.F.);
#2633=ORIENTED_EDGE('',*,*,#2104,.F.);
#2634=ORIENTED_EDGE('',*,*,#2105,.T.);
#2635=ORIENTED_EDGE('',*,*,#2106,.T.);
#2636=ORIENTED_EDGE('',*,*,#2105,.F.);
#2637=ORIENTED_EDGE('',*,*,#2106,.F.);
#2638=ORIENTED_EDGE('',*,*,#2087,.T.);
#2639=ORIENTED_EDGE('',*,*,#2090,.F.);
#2640=ORIENTED_EDGE('',*,*,#2088,.F.);
#2641=ORIENTED_EDGE('',*,*,#2107,.F.);
#2642=ORIENTED_EDGE('',*,*,#2108,.T.);
#2643=ORIENTED_EDGE('',*,*,#2109,.F.);
#2644=ORIENTED_EDGE('',*,*,#2108,.F.);
#2645=ORIENTED_EDGE('',*,*,#2092,.F.);
#2646=ORIENTED_EDGE('',*,*,#2107,.T.);
#2647=ORIENTED_EDGE('',*,*,#2110,.F.);
#2648=ORIENTED_EDGE('',*,*,#2111,.T.);
#2649=ORIENTED_EDGE('',*,*,#2078,.F.);
#2650=ORIENTED_EDGE('',*,*,#2074,.T.);
#2651=ORIENTED_EDGE('',*,*,#2080,.F.);
#2652=ORIENTED_EDGE('',*,*,#2112,.T.);
#2653=ORIENTED_EDGE('',*,*,#2113,.F.);
#2654=ORIENTED_EDGE('',*,*,#2112,.F.);
#2655=ORIENTED_EDGE('',*,*,#2075,.T.);
#2656=ORIENTED_EDGE('',*,*,#2072,.T.);
#2657=ORIENTED_EDGE('',*,*,#2077,.T.);
#2658=ORIENTED_EDGE('',*,*,#2111,.F.);
#2659=ORIENTED_EDGE('',*,*,#2110,.T.);
#2660=ORIENTED_EDGE('',*,*,#2109,.T.);
#2661=ORIENTED_EDGE('',*,*,#2114,.F.);
#2662=ORIENTED_EDGE('',*,*,#2115,.T.);
#2663=ORIENTED_EDGE('',*,*,#2095,.T.);
#2664=ORIENTED_EDGE('',*,*,#2116,.T.);
#2665=ORIENTED_EDGE('',*,*,#2117,.T.);
#2666=ORIENTED_EDGE('',*,*,#2116,.F.);
#2667=ORIENTED_EDGE('',*,*,#2094,.T.);
#2668=ORIENTED_EDGE('',*,*,#2093,.T.);
#2669=ORIENTED_EDGE('',*,*,#2115,.F.);
#2670=ORIENTED_EDGE('',*,*,#2082,.T.);
#2671=ORIENTED_EDGE('',*,*,#2083,.T.);
#2672=ORIENTED_EDGE('',*,*,#2114,.T.);
#2673=ORIENTED_EDGE('',*,*,#2113,.T.);
#2674=ORIENTED_EDGE('',*,*,#2070,.T.);
#2675=ORIENTED_EDGE('',*,*,#2067,.T.);
#2676=ORIENTED_EDGE('',*,*,#2064,.T.);
#2677=ORIENTED_EDGE('',*,*,#2061,.T.);
#2678=ORIENTED_EDGE('',*,*,#2058,.T.);
#2679=ORIENTED_EDGE('',*,*,#2055,.T.);
#2680=ORIENTED_EDGE('',*,*,#2117,.F.);
#2681=ORIENTED_EDGE('',*,*,#2098,.T.);
#2682=ORIENTED_EDGE('',*,*,#2101,.T.);
#2683=ORIENTED_EDGE('',*,*,#2104,.T.);
#2684=ORIENTED_EDGE('',*,*,#2118,.T.);
#2685=ORIENTED_EDGE('',*,*,#2119,.F.);
#2686=ORIENTED_EDGE('',*,*,#2118,.F.);
#2687=ORIENTED_EDGE('',*,*,#2120,.T.);
#2688=ORIENTED_EDGE('',*,*,#2121,.T.);
#2689=ORIENTED_EDGE('',*,*,#2120,.F.);
#2690=ORIENTED_EDGE('',*,*,#2121,.F.);
#2691=ORIENTED_EDGE('',*,*,#2122,.F.);
#2692=ORIENTED_EDGE('',*,*,#2123,.T.);
#2693=ORIENTED_EDGE('',*,*,#2119,.T.);
#2694=ORIENTED_EDGE('',*,*,#2123,.F.);
#2695=ORIENTED_EDGE('',*,*,#2122,.T.);
#2696=ORIENTED_EDGE('',*,*,#2124,.F.);
#2697=ORIENTED_EDGE('',*,*,#2125,.T.);
#2698=ORIENTED_EDGE('',*,*,#2126,.T.);
#2699=ORIENTED_EDGE('',*,*,#2125,.F.);
#2700=ORIENTED_EDGE('',*,*,#2127,.F.);
#2701=ORIENTED_EDGE('',*,*,#2128,.T.);
#2702=ORIENTED_EDGE('',*,*,#2129,.T.);
#2703=ORIENTED_EDGE('',*,*,#2128,.F.);
#2704=ORIENTED_EDGE('',*,*,#2127,.T.);
#2705=ORIENTED_EDGE('',*,*,#2124,.T.);
#2706=ORIENTED_EDGE('',*,*,#2129,.F.);
#2707=ORIENTED_EDGE('',*,*,#2126,.F.);
#2708=ORIENTED_EDGE('',*,*,#2130,.F.);
#2709=ORIENTED_EDGE('',*,*,#2131,.F.);
#2710=ORIENTED_EDGE('',*,*,#2132,.F.);
#2711=ORIENTED_EDGE('',*,*,#2133,.T.);
#2712=ORIENTED_EDGE('',*,*,#2130,.T.);
#2713=ORIENTED_EDGE('',*,*,#2133,.F.);
#2714=ORIENTED_EDGE('',*,*,#2134,.T.);
#2715=ORIENTED_EDGE('',*,*,#2135,.F.);
#2716=ORIENTED_EDGE('',*,*,#2136,.F.);
#2717=ORIENTED_EDGE('',*,*,#2137,.F.);
#2718=ORIENTED_EDGE('',*,*,#2134,.F.);
#2719=ORIENTED_EDGE('',*,*,#2138,.T.);
#2720=ORIENTED_EDGE('',*,*,#2136,.T.);
#2721=ORIENTED_EDGE('',*,*,#2138,.F.);
#2722=ORIENTED_EDGE('',*,*,#2137,.T.);
#2723=ORIENTED_EDGE('',*,*,#2139,.T.);
#2724=ORIENTED_EDGE('',*,*,#2140,.F.);
#2725=ORIENTED_EDGE('',*,*,#2139,.F.);
#2726=ORIENTED_EDGE('',*,*,#2131,.T.);
#2727=ORIENTED_EDGE('',*,*,#2141,.T.);
#2728=ORIENTED_EDGE('',*,*,#2135,.T.);
#2729=ORIENTED_EDGE('',*,*,#2141,.F.);
#2730=ORIENTED_EDGE('',*,*,#2132,.T.);
#2731=ORIENTED_EDGE('',*,*,#2142,.F.);
#2732=ORIENTED_EDGE('',*,*,#2143,.T.);
#2733=ORIENTED_EDGE('',*,*,#2144,.T.);
#2734=ORIENTED_EDGE('',*,*,#2143,.F.);
#2735=ORIENTED_EDGE('',*,*,#2142,.T.);
#2736=ORIENTED_EDGE('',*,*,#2140,.T.);
#2737=ORIENTED_EDGE('',*,*,#2144,.F.);
#2738=ORIENTED_EDGE('',*,*,#2145,.T.);
#2739=ORIENTED_EDGE('',*,*,#2146,.T.);
#2740=ORIENTED_EDGE('',*,*,#2147,.F.);
#2741=ORIENTED_EDGE('',*,*,#2146,.F.);
#2742=ORIENTED_EDGE('',*,*,#2147,.T.);
#2743=ORIENTED_EDGE('',*,*,#2145,.F.);
#2744=ORIENTED_EDGE('',*,*,#2148,.F.);
#2745=ORIENTED_EDGE('',*,*,#2149,.T.);
#2746=ORIENTED_EDGE('',*,*,#2150,.T.);
#2747=ORIENTED_EDGE('',*,*,#2149,.F.);
#2748=ORIENTED_EDGE('',*,*,#2151,.F.);
#2749=ORIENTED_EDGE('',*,*,#2152,.T.);
#2750=ORIENTED_EDGE('',*,*,#2153,.T.);
#2751=ORIENTED_EDGE('',*,*,#2152,.F.);
#2752=ORIENTED_EDGE('',*,*,#2151,.T.);
#2753=ORIENTED_EDGE('',*,*,#2148,.T.);
#2754=ORIENTED_EDGE('',*,*,#2153,.F.);
#2755=ORIENTED_EDGE('',*,*,#2150,.F.);
#2756=ORIENTED_EDGE('',*,*,#2154,.F.);
#2757=ORIENTED_EDGE('',*,*,#2155,.T.);
#2758=ORIENTED_EDGE('',*,*,#2156,.F.);
#2759=ORIENTED_EDGE('',*,*,#2155,.F.);
#2760=ORIENTED_EDGE('',*,*,#2157,.F.);
#2761=ORIENTED_EDGE('',*,*,#2158,.T.);
#2762=ORIENTED_EDGE('',*,*,#2159,.F.);
#2763=ORIENTED_EDGE('',*,*,#2158,.F.);
#2764=ORIENTED_EDGE('',*,*,#2160,.F.);
#2765=ORIENTED_EDGE('',*,*,#2161,.T.);
#2766=ORIENTED_EDGE('',*,*,#2162,.F.);
#2767=ORIENTED_EDGE('',*,*,#2161,.F.);
#2768=ORIENTED_EDGE('',*,*,#2163,.F.);
#2769=ORIENTED_EDGE('',*,*,#2164,.T.);
#2770=ORIENTED_EDGE('',*,*,#2165,.F.);
#2771=ORIENTED_EDGE('',*,*,#2164,.F.);
#2772=ORIENTED_EDGE('',*,*,#2166,.F.);
#2773=ORIENTED_EDGE('',*,*,#2167,.T.);
#2774=ORIENTED_EDGE('',*,*,#2168,.F.);
#2775=ORIENTED_EDGE('',*,*,#2167,.F.);
#2776=ORIENTED_EDGE('',*,*,#2169,.F.);
#2777=ORIENTED_EDGE('',*,*,#2170,.T.);
#2778=ORIENTED_EDGE('',*,*,#2171,.F.);
#2779=ORIENTED_EDGE('',*,*,#2170,.F.);
#2780=ORIENTED_EDGE('',*,*,#2172,.F.);
#2781=ORIENTED_EDGE('',*,*,#2173,.T.);
#2782=ORIENTED_EDGE('',*,*,#2174,.T.);
#2783=ORIENTED_EDGE('',*,*,#2173,.F.);
#2784=ORIENTED_EDGE('',*,*,#2175,.F.);
#2785=ORIENTED_EDGE('',*,*,#2176,.T.);
#2786=ORIENTED_EDGE('',*,*,#2177,.T.);
#2787=ORIENTED_EDGE('',*,*,#2176,.F.);
#2788=ORIENTED_EDGE('',*,*,#2175,.T.);
#2789=ORIENTED_EDGE('',*,*,#2172,.T.);
#2790=ORIENTED_EDGE('',*,*,#2171,.T.);
#2791=ORIENTED_EDGE('',*,*,#2168,.T.);
#2792=ORIENTED_EDGE('',*,*,#2165,.T.);
#2793=ORIENTED_EDGE('',*,*,#2162,.T.);
#2794=ORIENTED_EDGE('',*,*,#2159,.T.);
#2795=ORIENTED_EDGE('',*,*,#2156,.T.);
#2796=ORIENTED_EDGE('',*,*,#2177,.F.);
#2797=ORIENTED_EDGE('',*,*,#2174,.F.);
#2798=ORIENTED_EDGE('',*,*,#2169,.T.);
#2799=ORIENTED_EDGE('',*,*,#2166,.T.);
#2800=ORIENTED_EDGE('',*,*,#2163,.T.);
#2801=ORIENTED_EDGE('',*,*,#2160,.T.);
#2802=ORIENTED_EDGE('',*,*,#2157,.T.);
#2803=ORIENTED_EDGE('',*,*,#2154,.T.);
#2804=ORIENTED_EDGE('',*,*,#2178,.F.);
#2805=ORIENTED_EDGE('',*,*,#2179,.T.);
#2806=ORIENTED_EDGE('',*,*,#2180,.F.);
#2807=ORIENTED_EDGE('',*,*,#2179,.F.);
#2808=ORIENTED_EDGE('',*,*,#2181,.F.);
#2809=ORIENTED_EDGE('',*,*,#2182,.T.);
#2810=ORIENTED_EDGE('',*,*,#2183,.F.);
#2811=ORIENTED_EDGE('',*,*,#2182,.F.);
#2812=ORIENTED_EDGE('',*,*,#2181,.T.);
#2813=ORIENTED_EDGE('',*,*,#2178,.T.);
#2814=ORIENTED_EDGE('',*,*,#2184,.T.);
#2815=ORIENTED_EDGE('',*,*,#2183,.T.);
#2816=ORIENTED_EDGE('',*,*,#2185,.F.);
#2817=ORIENTED_EDGE('',*,*,#2186,.T.);
#2818=ORIENTED_EDGE('',*,*,#2187,.T.);
#2819=ORIENTED_EDGE('',*,*,#2186,.F.);
#2820=ORIENTED_EDGE('',*,*,#2184,.F.);
#2821=ORIENTED_EDGE('',*,*,#2188,.T.);
#2822=ORIENTED_EDGE('',*,*,#2189,.T.);
#2823=ORIENTED_EDGE('',*,*,#2188,.F.);
#2824=ORIENTED_EDGE('',*,*,#2180,.T.);
#2825=ORIENTED_EDGE('',*,*,#2185,.T.);
#2826=ORIENTED_EDGE('',*,*,#2189,.F.);
#2827=ORIENTED_EDGE('',*,*,#2187,.F.);
#2828=ORIENTED_EDGE('',*,*,#2190,.F.);
#2829=ORIENTED_EDGE('',*,*,#2191,.F.);
#2830=ORIENTED_EDGE('',*,*,#2192,.F.);
#2831=ORIENTED_EDGE('',*,*,#2193,.F.);
#2832=ORIENTED_EDGE('',*,*,#2194,.F.);
#2833=ORIENTED_EDGE('',*,*,#2191,.T.);
#2834=ORIENTED_EDGE('',*,*,#2195,.F.);
#2835=ORIENTED_EDGE('',*,*,#2196,.T.);
#2836=ORIENTED_EDGE('',*,*,#2197,.F.);
#2837=ORIENTED_EDGE('',*,*,#2198,.F.);
#2838=ORIENTED_EDGE('',*,*,#2199,.F.);
#2839=ORIENTED_EDGE('',*,*,#2196,.F.);
#2840=ORIENTED_EDGE('',*,*,#2200,.F.);
#2841=ORIENTED_EDGE('',*,*,#2201,.F.);
#2842=ORIENTED_EDGE('',*,*,#2202,.F.);
#2843=ORIENTED_EDGE('',*,*,#2203,.F.);
#2844=ORIENTED_EDGE('',*,*,#2204,.F.);
#2845=ORIENTED_EDGE('',*,*,#2201,.T.);
#2846=ORIENTED_EDGE('',*,*,#2205,.F.);
#2847=ORIENTED_EDGE('',*,*,#2206,.F.);
#2848=ORIENTED_EDGE('',*,*,#2207,.F.);
#2849=ORIENTED_EDGE('',*,*,#2208,.F.);
#2850=ORIENTED_EDGE('',*,*,#2209,.F.);
#2851=ORIENTED_EDGE('',*,*,#2206,.T.);
#2852=ORIENTED_EDGE('',*,*,#2210,.F.);
#2853=ORIENTED_EDGE('',*,*,#2211,.F.);
#2854=ORIENTED_EDGE('',*,*,#2212,.F.);
#2855=ORIENTED_EDGE('',*,*,#2213,.F.);
#2856=ORIENTED_EDGE('',*,*,#2214,.F.);
#2857=ORIENTED_EDGE('',*,*,#2211,.T.);
#2858=ORIENTED_EDGE('',*,*,#2215,.F.);
#2859=ORIENTED_EDGE('',*,*,#2216,.T.);
#2860=ORIENTED_EDGE('',*,*,#2217,.F.);
#2861=ORIENTED_EDGE('',*,*,#2218,.F.);
#2862=ORIENTED_EDGE('',*,*,#2219,.F.);
#2863=ORIENTED_EDGE('',*,*,#2216,.F.);
#2864=ORIENTED_EDGE('',*,*,#2220,.F.);
#2865=ORIENTED_EDGE('',*,*,#2221,.T.);
#2866=ORIENTED_EDGE('',*,*,#2222,.F.);
#2867=ORIENTED_EDGE('',*,*,#2212,.T.);
#2868=ORIENTED_EDGE('',*,*,#2210,.T.);
#2869=ORIENTED_EDGE('',*,*,#2214,.T.);
#2870=ORIENTED_EDGE('',*,*,#2223,.F.);
#2871=ORIENTED_EDGE('',*,*,#2192,.T.);
#2872=ORIENTED_EDGE('',*,*,#2190,.T.);
#2873=ORIENTED_EDGE('',*,*,#2194,.T.);
#2874=ORIENTED_EDGE('',*,*,#2224,.F.);
#2875=ORIENTED_EDGE('',*,*,#2217,.T.);
#2876=ORIENTED_EDGE('',*,*,#2219,.T.);
#2877=ORIENTED_EDGE('',*,*,#2215,.T.);
#2878=ORIENTED_EDGE('',*,*,#2225,.F.);
#2879=ORIENTED_EDGE('',*,*,#2197,.T.);
#2880=ORIENTED_EDGE('',*,*,#2199,.T.);
#2881=ORIENTED_EDGE('',*,*,#2195,.T.);
#2882=ORIENTED_EDGE('',*,*,#2226,.F.);
#2883=ORIENTED_EDGE('',*,*,#2202,.T.);
#2884=ORIENTED_EDGE('',*,*,#2200,.T.);
#2885=ORIENTED_EDGE('',*,*,#2204,.T.);
#2886=ORIENTED_EDGE('',*,*,#2227,.F.);
#2887=ORIENTED_EDGE('',*,*,#2207,.T.);
#2888=ORIENTED_EDGE('',*,*,#2205,.T.);
#2889=ORIENTED_EDGE('',*,*,#2209,.T.);
#2890=ORIENTED_EDGE('',*,*,#2228,.F.);
#2891=ORIENTED_EDGE('',*,*,#2221,.F.);
#2892=ORIENTED_EDGE('',*,*,#2229,.F.);
#2893=ORIENTED_EDGE('',*,*,#2230,.T.);
#2894=ORIENTED_EDGE('',*,*,#2231,.F.);
#2895=ORIENTED_EDGE('',*,*,#2230,.F.);
#2896=ORIENTED_EDGE('',*,*,#2232,.F.);
#2897=ORIENTED_EDGE('',*,*,#2233,.T.);
#2898=ORIENTED_EDGE('',*,*,#2234,.F.);
#2899=ORIENTED_EDGE('',*,*,#2233,.F.);
#2900=ORIENTED_EDGE('',*,*,#2235,.F.);
#2901=ORIENTED_EDGE('',*,*,#2236,.T.);
#2902=ORIENTED_EDGE('',*,*,#2237,.F.);
#2903=ORIENTED_EDGE('',*,*,#2236,.F.);
#2904=ORIENTED_EDGE('',*,*,#2238,.F.);
#2905=ORIENTED_EDGE('',*,*,#2239,.T.);
#2906=ORIENTED_EDGE('',*,*,#2240,.F.);
#2907=ORIENTED_EDGE('',*,*,#2239,.F.);
#2908=ORIENTED_EDGE('',*,*,#2241,.F.);
#2909=ORIENTED_EDGE('',*,*,#2242,.T.);
#2910=ORIENTED_EDGE('',*,*,#2243,.F.);
#2911=ORIENTED_EDGE('',*,*,#2242,.F.);
#2912=ORIENTED_EDGE('',*,*,#2244,.F.);
#2913=ORIENTED_EDGE('',*,*,#2245,.T.);
#2914=ORIENTED_EDGE('',*,*,#2246,.F.);
#2915=ORIENTED_EDGE('',*,*,#2245,.F.);
#2916=ORIENTED_EDGE('',*,*,#2247,.F.);
#2917=ORIENTED_EDGE('',*,*,#2248,.T.);
#2918=ORIENTED_EDGE('',*,*,#2249,.F.);
#2919=ORIENTED_EDGE('',*,*,#2248,.F.);
#2920=ORIENTED_EDGE('',*,*,#2250,.F.);
#2921=ORIENTED_EDGE('',*,*,#2251,.T.);
#2922=ORIENTED_EDGE('',*,*,#2252,.T.);
#2923=ORIENTED_EDGE('',*,*,#2251,.F.);
#2924=ORIENTED_EDGE('',*,*,#2252,.F.);
#2925=ORIENTED_EDGE('',*,*,#2247,.T.);
#2926=ORIENTED_EDGE('',*,*,#2220,.T.);
#2927=ORIENTED_EDGE('',*,*,#2249,.T.);
#2928=ORIENTED_EDGE('',*,*,#2253,.F.);
#2929=ORIENTED_EDGE('',*,*,#2254,.T.);
#2930=ORIENTED_EDGE('',*,*,#2255,.T.);
#2931=ORIENTED_EDGE('',*,*,#2254,.F.);
#2932=ORIENTED_EDGE('',*,*,#2253,.T.);
#2933=ORIENTED_EDGE('',*,*,#2231,.T.);
#2934=ORIENTED_EDGE('',*,*,#2234,.T.);
#2935=ORIENTED_EDGE('',*,*,#2237,.T.);
#2936=ORIENTED_EDGE('',*,*,#2240,.T.);
#2937=ORIENTED_EDGE('',*,*,#2243,.T.);
#2938=ORIENTED_EDGE('',*,*,#2246,.T.);
#2939=ORIENTED_EDGE('',*,*,#2223,.T.);
#2940=ORIENTED_EDGE('',*,*,#2213,.T.);
#2941=ORIENTED_EDGE('',*,*,#2222,.T.);
#2942=ORIENTED_EDGE('',*,*,#2228,.T.);
#2943=ORIENTED_EDGE('',*,*,#2208,.T.);
#2944=ORIENTED_EDGE('',*,*,#2227,.T.);
#2945=ORIENTED_EDGE('',*,*,#2203,.T.);
#2946=ORIENTED_EDGE('',*,*,#2226,.T.);
#2947=ORIENTED_EDGE('',*,*,#2198,.T.);
#2948=ORIENTED_EDGE('',*,*,#2225,.T.);
#2949=ORIENTED_EDGE('',*,*,#2218,.T.);
#2950=ORIENTED_EDGE('',*,*,#2224,.T.);
#2951=ORIENTED_EDGE('',*,*,#2193,.T.);
#2952=ORIENTED_EDGE('',*,*,#2255,.F.);
#2953=ORIENTED_EDGE('',*,*,#2250,.T.);
#2954=ORIENTED_EDGE('',*,*,#2244,.T.);
#2955=ORIENTED_EDGE('',*,*,#2241,.T.);
#2956=ORIENTED_EDGE('',*,*,#2238,.T.);
#2957=ORIENTED_EDGE('',*,*,#2235,.T.);
#2958=ORIENTED_EDGE('',*,*,#2232,.T.);
#2959=ORIENTED_EDGE('',*,*,#2229,.T.);
#2960=ORIENTED_EDGE('',*,*,#2256,.T.);
#2961=ORIENTED_EDGE('',*,*,#2257,.T.);
#2962=ORIENTED_EDGE('',*,*,#2258,.F.);
#2963=ORIENTED_EDGE('',*,*,#2257,.F.);
#2964=ORIENTED_EDGE('',*,*,#2258,.T.);
#2965=ORIENTED_EDGE('',*,*,#2256,.F.);
#2966=ORIENTED_EDGE('',*,*,#2259,.F.);
#2967=ORIENTED_EDGE('',*,*,#2260,.T.);
#2968=ORIENTED_EDGE('',*,*,#2261,.T.);
#2969=ORIENTED_EDGE('',*,*,#2260,.F.);
#2970=ORIENTED_EDGE('',*,*,#2261,.F.);
#2971=ORIENTED_EDGE('',*,*,#2262,.F.);
#2972=ORIENTED_EDGE('',*,*,#2263,.T.);
#2973=ORIENTED_EDGE('',*,*,#2264,.T.);
#2974=ORIENTED_EDGE('',*,*,#2263,.F.);
#2975=ORIENTED_EDGE('',*,*,#2262,.T.);
#2976=ORIENTED_EDGE('',*,*,#2264,.F.);
#2977=ORIENTED_EDGE('',*,*,#2259,.T.);
#2978=ORIENTED_EDGE('',*,*,#2265,.F.);
#2979=ORIENTED_EDGE('',*,*,#2266,.T.);
#2980=ORIENTED_EDGE('',*,*,#2267,.T.);
#2981=ORIENTED_EDGE('',*,*,#2266,.F.);
#2982=ORIENTED_EDGE('',*,*,#2265,.T.);
#2983=ORIENTED_EDGE('',*,*,#2267,.F.);
#2984=ORIENTED_EDGE('',*,*,#2268,.F.);
#2985=ORIENTED_EDGE('',*,*,#2269,.T.);
#2986=ORIENTED_EDGE('',*,*,#2270,.T.);
#2987=ORIENTED_EDGE('',*,*,#2271,.F.);
#2988=ORIENTED_EDGE('',*,*,#2272,.F.);
#2989=ORIENTED_EDGE('',*,*,#2273,.F.);
#2990=ORIENTED_EDGE('',*,*,#2270,.F.);
#2991=ORIENTED_EDGE('',*,*,#2274,.T.);
#2992=ORIENTED_EDGE('',*,*,#2275,.F.);
#2993=ORIENTED_EDGE('',*,*,#2274,.F.);
#2994=ORIENTED_EDGE('',*,*,#2269,.F.);
#2995=ORIENTED_EDGE('',*,*,#2276,.F.);
#2996=ORIENTED_EDGE('',*,*,#2272,.T.);
#2997=ORIENTED_EDGE('',*,*,#2277,.F.);
#2998=ORIENTED_EDGE('',*,*,#2278,.T.);
#2999=ORIENTED_EDGE('',*,*,#2279,.T.);
#3000=ORIENTED_EDGE('',*,*,#2278,.F.);
#3001=ORIENTED_EDGE('',*,*,#2273,.T.);
#3002=ORIENTED_EDGE('',*,*,#2276,.T.);
#3003=ORIENTED_EDGE('',*,*,#2271,.T.);
#3004=ORIENTED_EDGE('',*,*,#2268,.T.);
#3005=ORIENTED_EDGE('',*,*,#2280,.F.);
#3006=ORIENTED_EDGE('',*,*,#2281,.T.);
#3007=ORIENTED_EDGE('',*,*,#2282,.T.);
#3008=ORIENTED_EDGE('',*,*,#2281,.F.);
#3009=ORIENTED_EDGE('',*,*,#2275,.T.);
#3010=ORIENTED_EDGE('',*,*,#2280,.T.);
#3011=ORIENTED_EDGE('',*,*,#2277,.T.);
#3012=ORIENTED_EDGE('',*,*,#2282,.F.);
#3013=ORIENTED_EDGE('',*,*,#2279,.F.);
#3014=ORIENTED_EDGE('',*,*,#2283,.T.);
#3015=ORIENTED_EDGE('',*,*,#2284,.T.);
#3016=ORIENTED_EDGE('',*,*,#2285,.F.);
#3017=ORIENTED_EDGE('',*,*,#2286,.F.);
#3018=ORIENTED_EDGE('',*,*,#2287,.T.);
#3019=ORIENTED_EDGE('',*,*,#2286,.T.);
#3020=ORIENTED_EDGE('',*,*,#2288,.F.);
#3021=ORIENTED_EDGE('',*,*,#2289,.F.);
#3022=ORIENTED_EDGE('',*,*,#2290,.T.);
#3023=ORIENTED_EDGE('',*,*,#2289,.T.);
#3024=ORIENTED_EDGE('',*,*,#2291,.F.);
#3025=ORIENTED_EDGE('',*,*,#2292,.F.);
#3026=ORIENTED_EDGE('',*,*,#2293,.T.);
#3027=ORIENTED_EDGE('',*,*,#2292,.T.);
#3028=ORIENTED_EDGE('',*,*,#2294,.F.);
#3029=ORIENTED_EDGE('',*,*,#2284,.F.);
#3030=ORIENTED_EDGE('',*,*,#2294,.T.);
#3031=ORIENTED_EDGE('',*,*,#2291,.T.);
#3032=ORIENTED_EDGE('',*,*,#2288,.T.);
#3033=ORIENTED_EDGE('',*,*,#2285,.T.);
#3034=ORIENTED_EDGE('',*,*,#2293,.F.);
#3035=ORIENTED_EDGE('',*,*,#2283,.F.);
#3036=ORIENTED_EDGE('',*,*,#2287,.F.);
#3037=ORIENTED_EDGE('',*,*,#2290,.F.);
#3038=ORIENTED_EDGE('',*,*,#2295,.T.);
#3039=ORIENTED_EDGE('',*,*,#2296,.T.);
#3040=ORIENTED_EDGE('',*,*,#2297,.F.);
#3041=ORIENTED_EDGE('',*,*,#2298,.F.);
#3042=ORIENTED_EDGE('',*,*,#2299,.T.);
#3043=ORIENTED_EDGE('',*,*,#2298,.T.);
#3044=ORIENTED_EDGE('',*,*,#2300,.F.);
#3045=ORIENTED_EDGE('',*,*,#2301,.F.);
#3046=ORIENTED_EDGE('',*,*,#2302,.T.);
#3047=ORIENTED_EDGE('',*,*,#2301,.T.);
#3048=ORIENTED_EDGE('',*,*,#2303,.F.);
#3049=ORIENTED_EDGE('',*,*,#2304,.F.);
#3050=ORIENTED_EDGE('',*,*,#2305,.T.);
#3051=ORIENTED_EDGE('',*,*,#2304,.T.);
#3052=ORIENTED_EDGE('',*,*,#2306,.F.);
#3053=ORIENTED_EDGE('',*,*,#2296,.F.);
#3054=ORIENTED_EDGE('',*,*,#2306,.T.);
#3055=ORIENTED_EDGE('',*,*,#2303,.T.);
#3056=ORIENTED_EDGE('',*,*,#2300,.T.);
#3057=ORIENTED_EDGE('',*,*,#2297,.T.);
#3058=ORIENTED_EDGE('',*,*,#2305,.F.);
#3059=ORIENTED_EDGE('',*,*,#2295,.F.);
#3060=ORIENTED_EDGE('',*,*,#2299,.F.);
#3061=ORIENTED_EDGE('',*,*,#2302,.F.);
#3062=ORIENTED_EDGE('',*,*,#2307,.F.);
#3063=ORIENTED_EDGE('',*,*,#2308,.F.);
#3064=ORIENTED_EDGE('',*,*,#2309,.T.);
#3065=ORIENTED_EDGE('',*,*,#2307,.T.);
#3066=ORIENTED_EDGE('',*,*,#2309,.F.);
#3067=ORIENTED_EDGE('',*,*,#2310,.F.);
#3068=ORIENTED_EDGE('',*,*,#2311,.T.);
#3069=ORIENTED_EDGE('',*,*,#2308,.T.);
#3070=ORIENTED_EDGE('',*,*,#2311,.F.);
#3071=ORIENTED_EDGE('',*,*,#2312,.F.);
#3072=ORIENTED_EDGE('',*,*,#2313,.T.);
#3073=ORIENTED_EDGE('',*,*,#2310,.T.);
#3074=ORIENTED_EDGE('',*,*,#2313,.F.);
#3075=ORIENTED_EDGE('',*,*,#2312,.T.);
#3076=ORIENTED_EDGE('',*,*,#2314,.F.);
#3077=ORIENTED_EDGE('',*,*,#2315,.F.);
#3078=ORIENTED_EDGE('',*,*,#2316,.T.);
#3079=ORIENTED_EDGE('',*,*,#2314,.T.);
#3080=ORIENTED_EDGE('',*,*,#2316,.F.);
#3081=ORIENTED_EDGE('',*,*,#2317,.F.);
#3082=ORIENTED_EDGE('',*,*,#2318,.T.);
#3083=ORIENTED_EDGE('',*,*,#2315,.T.);
#3084=ORIENTED_EDGE('',*,*,#2318,.F.);
#3085=ORIENTED_EDGE('',*,*,#2319,.F.);
#3086=ORIENTED_EDGE('',*,*,#2320,.T.);
#3087=ORIENTED_EDGE('',*,*,#2317,.T.);
#3088=ORIENTED_EDGE('',*,*,#2320,.F.);
#3089=ORIENTED_EDGE('',*,*,#2319,.T.);
#3090=ORIENTED_EDGE('',*,*,#2321,.T.);
#3091=ORIENTED_EDGE('',*,*,#2322,.T.);
#3092=ORIENTED_EDGE('',*,*,#2323,.T.);
#3093=ORIENTED_EDGE('',*,*,#2324,.F.);
#3094=ORIENTED_EDGE('',*,*,#2325,.T.);
#3095=ORIENTED_EDGE('',*,*,#2326,.T.);
#3096=ORIENTED_EDGE('',*,*,#2327,.T.);
#3097=ORIENTED_EDGE('',*,*,#2322,.F.);
#3098=ORIENTED_EDGE('',*,*,#2328,.T.);
#3099=ORIENTED_EDGE('',*,*,#2329,.T.);
#3100=ORIENTED_EDGE('',*,*,#2330,.T.);
#3101=ORIENTED_EDGE('',*,*,#2326,.F.);
#3102=ORIENTED_EDGE('',*,*,#2331,.T.);
#3103=ORIENTED_EDGE('',*,*,#2332,.T.);
#3104=ORIENTED_EDGE('',*,*,#2333,.T.);
#3105=ORIENTED_EDGE('',*,*,#2329,.F.);
#3106=ORIENTED_EDGE('',*,*,#2334,.T.);
#3107=ORIENTED_EDGE('',*,*,#2335,.T.);
#3108=ORIENTED_EDGE('',*,*,#2336,.T.);
#3109=ORIENTED_EDGE('',*,*,#2332,.F.);
#3110=ORIENTED_EDGE('',*,*,#2337,.T.);
#3111=ORIENTED_EDGE('',*,*,#2324,.T.);
#3112=ORIENTED_EDGE('',*,*,#2338,.T.);
#3113=ORIENTED_EDGE('',*,*,#2335,.F.);
#3114=ORIENTED_EDGE('',*,*,#2337,.F.);
#3115=ORIENTED_EDGE('',*,*,#2334,.F.);
#3116=ORIENTED_EDGE('',*,*,#2331,.F.);
#3117=ORIENTED_EDGE('',*,*,#2328,.F.);
#3118=ORIENTED_EDGE('',*,*,#2325,.F.);
#3119=ORIENTED_EDGE('',*,*,#2321,.F.);
#3120=ORIENTED_EDGE('',*,*,#2338,.F.);
#3121=ORIENTED_EDGE('',*,*,#2323,.F.);
#3122=ORIENTED_EDGE('',*,*,#2327,.F.);
#3123=ORIENTED_EDGE('',*,*,#2330,.F.);
#3124=ORIENTED_EDGE('',*,*,#2333,.F.);
#3125=ORIENTED_EDGE('',*,*,#2336,.F.);
#3126=ORIENTED_EDGE('',*,*,#2339,.T.);
#3127=ORIENTED_EDGE('',*,*,#2340,.T.);
#3128=ORIENTED_EDGE('',*,*,#2341,.T.);
#3129=ORIENTED_EDGE('',*,*,#2342,.T.);
#3130=ORIENTED_EDGE('',*,*,#2343,.T.);
#3131=ORIENTED_EDGE('',*,*,#2344,.T.);
#3132=ORIENTED_EDGE('',*,*,#2345,.F.);
#3133=ORIENTED_EDGE('',*,*,#2346,.T.);
#3134=ORIENTED_EDGE('',*,*,#2347,.T.);
#3135=ORIENTED_EDGE('',*,*,#2348,.T.);
#3136=ORIENTED_EDGE('',*,*,#2349,.T.);
#3137=ORIENTED_EDGE('',*,*,#2350,.T.);
#3138=ORIENTED_EDGE('',*,*,#2351,.T.);
#3139=ORIENTED_EDGE('',*,*,#2352,.F.);
#3140=ORIENTED_EDGE('',*,*,#2353,.F.);
#3141=ORIENTED_EDGE('',*,*,#2351,.F.);
#3142=ORIENTED_EDGE('',*,*,#2354,.F.);
#3143=ORIENTED_EDGE('',*,*,#2340,.F.);
#3144=ORIENTED_EDGE('',*,*,#2354,.T.);
#3145=ORIENTED_EDGE('',*,*,#2350,.F.);
#3146=ORIENTED_EDGE('',*,*,#2355,.F.);
#3147=ORIENTED_EDGE('',*,*,#2341,.F.);
#3148=ORIENTED_EDGE('',*,*,#2355,.T.);
#3149=ORIENTED_EDGE('',*,*,#2349,.F.);
#3150=ORIENTED_EDGE('',*,*,#2356,.F.);
#3151=ORIENTED_EDGE('',*,*,#2342,.F.);
#3152=ORIENTED_EDGE('',*,*,#2356,.T.);
#3153=ORIENTED_EDGE('',*,*,#2348,.F.);
#3154=ORIENTED_EDGE('',*,*,#2357,.F.);
#3155=ORIENTED_EDGE('',*,*,#2343,.F.);
#3156=ORIENTED_EDGE('',*,*,#2357,.T.);
#3157=ORIENTED_EDGE('',*,*,#2347,.F.);
#3158=ORIENTED_EDGE('',*,*,#2358,.F.);
#3159=ORIENTED_EDGE('',*,*,#2344,.F.);
#3160=ORIENTED_EDGE('',*,*,#2358,.T.);
#3161=ORIENTED_EDGE('',*,*,#2346,.F.);
#3162=ORIENTED_EDGE('',*,*,#2353,.T.);
#3163=ORIENTED_EDGE('',*,*,#2339,.F.);
#3164=ORIENTED_EDGE('',*,*,#2352,.T.);
#3165=ORIENTED_EDGE('',*,*,#2359,.T.);
#3166=ORIENTED_EDGE('',*,*,#2360,.T.);
#3167=ORIENTED_EDGE('',*,*,#2359,.F.);
#3168=ORIENTED_EDGE('',*,*,#2361,.F.);
#3169=ORIENTED_EDGE('',*,*,#2362,.T.);
#3170=ORIENTED_EDGE('',*,*,#2360,.F.);
#3171=ORIENTED_EDGE('',*,*,#2363,.T.);
#3172=ORIENTED_EDGE('',*,*,#2361,.T.);
#3173=ORIENTED_EDGE('',*,*,#2363,.F.);
#3174=ORIENTED_EDGE('',*,*,#2364,.F.);
#3175=ORIENTED_EDGE('',*,*,#2365,.T.);
#3176=ORIENTED_EDGE('',*,*,#2345,.T.);
#3177=ORIENTED_EDGE('',*,*,#2365,.F.);
#3178=ORIENTED_EDGE('',*,*,#2366,.F.);
#3179=ORIENTED_EDGE('',*,*,#2367,.T.);
#3180=ORIENTED_EDGE('',*,*,#2364,.T.);
#3181=ORIENTED_EDGE('',*,*,#2367,.F.);
#3182=ORIENTED_EDGE('',*,*,#2366,.T.);
#3183=ORIENTED_EDGE('',*,*,#2368,.F.);
#3184=ORIENTED_EDGE('',*,*,#2368,.T.);
#3185=ORIENTED_EDGE('',*,*,#2369,.T.);
#3186=ORIENTED_EDGE('',*,*,#2362,.F.);
#3187=ORIENTED_EDGE('',*,*,#2369,.F.);
#3188=ORIENTED_EDGE('',*,*,#2370,.F.);
#3189=ORIENTED_EDGE('',*,*,#2371,.F.);
#3190=ORIENTED_EDGE('',*,*,#2372,.T.);
#3191=ORIENTED_EDGE('',*,*,#2370,.T.);
#3192=ORIENTED_EDGE('',*,*,#2372,.F.);
#3193=ORIENTED_EDGE('',*,*,#2373,.F.);
#3194=ORIENTED_EDGE('',*,*,#2374,.T.);
#3195=ORIENTED_EDGE('',*,*,#2371,.T.);
#3196=ORIENTED_EDGE('',*,*,#2374,.F.);
#3197=ORIENTED_EDGE('',*,*,#2375,.F.);
#3198=ORIENTED_EDGE('',*,*,#2376,.T.);
#3199=ORIENTED_EDGE('',*,*,#2373,.T.);
#3200=ORIENTED_EDGE('',*,*,#2376,.F.);
#3201=ORIENTED_EDGE('',*,*,#2375,.T.);
#3202=ORIENTED_EDGE('',*,*,#2377,.F.);
#3203=ORIENTED_EDGE('',*,*,#2378,.F.);
#3204=ORIENTED_EDGE('',*,*,#2379,.T.);
#3205=ORIENTED_EDGE('',*,*,#2377,.T.);
#3206=ORIENTED_EDGE('',*,*,#2379,.F.);
#3207=ORIENTED_EDGE('',*,*,#2380,.F.);
#3208=ORIENTED_EDGE('',*,*,#2381,.T.);
#3209=ORIENTED_EDGE('',*,*,#2378,.T.);
#3210=ORIENTED_EDGE('',*,*,#2381,.F.);
#3211=ORIENTED_EDGE('',*,*,#2382,.F.);
#3212=ORIENTED_EDGE('',*,*,#2383,.T.);
#3213=ORIENTED_EDGE('',*,*,#2380,.T.);
#3214=ORIENTED_EDGE('',*,*,#2383,.F.);
#3215=ORIENTED_EDGE('',*,*,#2382,.T.);
#3216=ORIENTED_EDGE('',*,*,#2384,.T.);
#3217=ORIENTED_EDGE('',*,*,#2385,.T.);
#3218=ORIENTED_EDGE('',*,*,#2386,.T.);
#3219=ORIENTED_EDGE('',*,*,#2387,.F.);
#3220=ORIENTED_EDGE('',*,*,#2388,.T.);
#3221=ORIENTED_EDGE('',*,*,#2389,.T.);
#3222=ORIENTED_EDGE('',*,*,#2390,.T.);
#3223=ORIENTED_EDGE('',*,*,#2385,.F.);
#3224=ORIENTED_EDGE('',*,*,#2391,.T.);
#3225=ORIENTED_EDGE('',*,*,#2392,.T.);
#3226=ORIENTED_EDGE('',*,*,#2393,.T.);
#3227=ORIENTED_EDGE('',*,*,#2389,.F.);
#3228=ORIENTED_EDGE('',*,*,#2394,.T.);
#3229=ORIENTED_EDGE('',*,*,#2395,.T.);
#3230=ORIENTED_EDGE('',*,*,#2396,.T.);
#3231=ORIENTED_EDGE('',*,*,#2392,.F.);
#3232=ORIENTED_EDGE('',*,*,#2397,.T.);
#3233=ORIENTED_EDGE('',*,*,#2398,.T.);
#3234=ORIENTED_EDGE('',*,*,#2399,.T.);
#3235=ORIENTED_EDGE('',*,*,#2395,.F.);
#3236=ORIENTED_EDGE('',*,*,#2400,.T.);
#3237=ORIENTED_EDGE('',*,*,#2387,.T.);
#3238=ORIENTED_EDGE('',*,*,#2401,.T.);
#3239=ORIENTED_EDGE('',*,*,#2398,.F.);
#3240=ORIENTED_EDGE('',*,*,#2400,.F.);
#3241=ORIENTED_EDGE('',*,*,#2397,.F.);
#3242=ORIENTED_EDGE('',*,*,#2394,.F.);
#3243=ORIENTED_EDGE('',*,*,#2391,.F.);
#3244=ORIENTED_EDGE('',*,*,#2388,.F.);
#3245=ORIENTED_EDGE('',*,*,#2384,.F.);
#3246=ORIENTED_EDGE('',*,*,#2401,.F.);
#3247=ORIENTED_EDGE('',*,*,#2386,.F.);
#3248=ORIENTED_EDGE('',*,*,#2390,.F.);
#3249=ORIENTED_EDGE('',*,*,#2393,.F.);
#3250=ORIENTED_EDGE('',*,*,#2396,.F.);
#3251=ORIENTED_EDGE('',*,*,#2399,.F.);
#3252=ORIENTED_EDGE('',*,*,#2402,.F.);
#3253=ORIENTED_EDGE('',*,*,#2403,.T.);
#3254=ORIENTED_EDGE('',*,*,#2404,.T.);
#3255=ORIENTED_EDGE('',*,*,#2403,.F.);
#3256=ORIENTED_EDGE('',*,*,#2405,.F.);
#3257=ORIENTED_EDGE('',*,*,#2406,.T.);
#3258=ORIENTED_EDGE('',*,*,#2407,.T.);
#3259=ORIENTED_EDGE('',*,*,#2406,.F.);
#3260=ORIENTED_EDGE('',*,*,#2405,.T.);
#3261=ORIENTED_EDGE('',*,*,#2402,.T.);
#3262=ORIENTED_EDGE('',*,*,#2407,.F.);
#3263=ORIENTED_EDGE('',*,*,#2404,.F.);
#3264=ORIENTED_EDGE('',*,*,#2408,.F.);
#3265=ORIENTED_EDGE('',*,*,#2409,.F.);
#3266=ORIENTED_EDGE('',*,*,#2410,.T.);
#3267=ORIENTED_EDGE('',*,*,#2411,.F.);
#3268=ORIENTED_EDGE('',*,*,#2410,.F.);
#3269=ORIENTED_EDGE('',*,*,#2412,.F.);
#3270=ORIENTED_EDGE('',*,*,#2413,.F.);
#3271=ORIENTED_EDGE('',*,*,#2414,.F.);
#3272=ORIENTED_EDGE('',*,*,#2415,.F.);
#3273=ORIENTED_EDGE('',*,*,#2416,.F.);
#3274=ORIENTED_EDGE('',*,*,#2417,.T.);
#3275=ORIENTED_EDGE('',*,*,#2418,.F.);
#3276=ORIENTED_EDGE('',*,*,#2419,.F.);
#3277=ORIENTED_EDGE('',*,*,#2420,.F.);
#3278=ORIENTED_EDGE('',*,*,#2421,.F.);
#3279=ORIENTED_EDGE('',*,*,#2422,.F.);
#3280=ORIENTED_EDGE('',*,*,#2423,.F.);
#3281=ORIENTED_EDGE('',*,*,#2417,.F.);
#3282=ORIENTED_EDGE('',*,*,#2413,.T.);
#3283=ORIENTED_EDGE('',*,*,#2424,.T.);
#3284=ORIENTED_EDGE('',*,*,#2422,.T.);
#3285=ORIENTED_EDGE('',*,*,#2425,.F.);
#3286=ORIENTED_EDGE('',*,*,#2412,.T.);
#3287=ORIENTED_EDGE('',*,*,#2426,.T.);
#3288=ORIENTED_EDGE('',*,*,#2423,.T.);
#3289=ORIENTED_EDGE('',*,*,#2424,.F.);
#3290=ORIENTED_EDGE('',*,*,#2409,.T.);
#3291=ORIENTED_EDGE('',*,*,#2427,.T.);
#3292=ORIENTED_EDGE('',*,*,#2418,.T.);
#3293=ORIENTED_EDGE('',*,*,#2426,.F.);
#3294=ORIENTED_EDGE('',*,*,#2428,.F.);
#3295=ORIENTED_EDGE('',*,*,#2429,.T.);
#3296=ORIENTED_EDGE('',*,*,#2430,.T.);
#3297=ORIENTED_EDGE('',*,*,#2429,.F.);
#3298=ORIENTED_EDGE('',*,*,#2408,.T.);
#3299=ORIENTED_EDGE('',*,*,#2431,.T.);
#3300=ORIENTED_EDGE('',*,*,#2419,.T.);
#3301=ORIENTED_EDGE('',*,*,#2427,.F.);
#3302=ORIENTED_EDGE('',*,*,#2414,.T.);
#3303=ORIENTED_EDGE('',*,*,#2425,.T.);
#3304=ORIENTED_EDGE('',*,*,#2421,.T.);
#3305=ORIENTED_EDGE('',*,*,#2432,.F.);
#3306=ORIENTED_EDGE('',*,*,#2415,.T.);
#3307=ORIENTED_EDGE('',*,*,#2432,.T.);
#3308=ORIENTED_EDGE('',*,*,#2420,.T.);
#3309=ORIENTED_EDGE('',*,*,#2431,.F.);
#3310=ORIENTED_EDGE('',*,*,#2416,.T.);
#3311=ORIENTED_EDGE('',*,*,#2428,.T.);
#3312=ORIENTED_EDGE('',*,*,#2411,.T.);
#3313=ORIENTED_EDGE('',*,*,#2430,.F.);
#3314=ORIENTED_EDGE('',*,*,#2433,.F.);
#3315=ORIENTED_EDGE('',*,*,#2434,.T.);
#3316=ORIENTED_EDGE('',*,*,#2435,.T.);
#3317=ORIENTED_EDGE('',*,*,#2436,.F.);
#3318=ORIENTED_EDGE('',*,*,#2437,.F.);
#3319=ORIENTED_EDGE('',*,*,#2438,.T.);
#3320=ORIENTED_EDGE('',*,*,#2439,.T.);
#3321=ORIENTED_EDGE('',*,*,#2434,.F.);
#3322=ORIENTED_EDGE('',*,*,#2440,.F.);
#3323=ORIENTED_EDGE('',*,*,#2441,.T.);
#3324=ORIENTED_EDGE('',*,*,#2442,.T.);
#3325=ORIENTED_EDGE('',*,*,#2438,.F.);
#3326=ORIENTED_EDGE('',*,*,#2443,.F.);
#3327=ORIENTED_EDGE('',*,*,#2444,.T.);
#3328=ORIENTED_EDGE('',*,*,#2445,.T.);
#3329=ORIENTED_EDGE('',*,*,#2441,.F.);
#3330=ORIENTED_EDGE('',*,*,#2446,.F.);
#3331=ORIENTED_EDGE('',*,*,#2447,.T.);
#3332=ORIENTED_EDGE('',*,*,#2448,.T.);
#3333=ORIENTED_EDGE('',*,*,#2444,.F.);
#3334=ORIENTED_EDGE('',*,*,#2449,.F.);
#3335=ORIENTED_EDGE('',*,*,#2436,.T.);
#3336=ORIENTED_EDGE('',*,*,#2450,.T.);
#3337=ORIENTED_EDGE('',*,*,#2447,.F.);
#3338=ORIENTED_EDGE('',*,*,#2450,.F.);
#3339=ORIENTED_EDGE('',*,*,#2435,.F.);
#3340=ORIENTED_EDGE('',*,*,#2439,.F.);
#3341=ORIENTED_EDGE('',*,*,#2442,.F.);
#3342=ORIENTED_EDGE('',*,*,#2445,.F.);
#3343=ORIENTED_EDGE('',*,*,#2448,.F.);
#3344=ORIENTED_EDGE('',*,*,#2451,.F.);
#3345=ORIENTED_EDGE('',*,*,#2433,.T.);
#3346=ORIENTED_EDGE('',*,*,#2449,.T.);
#3347=ORIENTED_EDGE('',*,*,#2446,.T.);
#3348=ORIENTED_EDGE('',*,*,#2443,.T.);
#3349=ORIENTED_EDGE('',*,*,#2440,.T.);
#3350=ORIENTED_EDGE('',*,*,#2437,.T.);
#3351=ORIENTED_EDGE('',*,*,#2452,.F.);
#3352=ORIENTED_EDGE('',*,*,#2453,.T.);
#3353=ORIENTED_EDGE('',*,*,#2451,.T.);
#3354=ORIENTED_EDGE('',*,*,#2453,.F.);
#3355=ORIENTED_EDGE('',*,*,#2454,.F.);
#3356=ORIENTED_EDGE('',*,*,#2455,.T.);
#3357=ORIENTED_EDGE('',*,*,#2452,.T.);
#3358=ORIENTED_EDGE('',*,*,#2455,.F.);
#3359=ORIENTED_EDGE('',*,*,#2456,.F.);
#3360=ORIENTED_EDGE('',*,*,#2457,.T.);
#3361=ORIENTED_EDGE('',*,*,#2454,.T.);
#3362=ORIENTED_EDGE('',*,*,#2457,.F.);
#3363=ORIENTED_EDGE('',*,*,#2456,.T.);
#3364=CYLINDRICAL_SURFACE('',#3968,0.225);
#3365=CYLINDRICAL_SURFACE('',#3971,0.225);
#3366=CYLINDRICAL_SURFACE('',#3981,0.225);
#3367=CYLINDRICAL_SURFACE('',#3991,0.225);
#3368=CYLINDRICAL_SURFACE('',#4001,0.21);
#3369=CYLINDRICAL_SURFACE('',#4005,0.21);
#3370=CYLINDRICAL_SURFACE('',#4009,0.21);
#3371=CYLINDRICAL_SURFACE('',#4013,0.21);
#3372=CYLINDRICAL_SURFACE('',#4017,0.21);
#3373=CYLINDRICAL_SURFACE('',#4021,0.21);
#3374=CYLINDRICAL_SURFACE('',#4025,0.4);
#3375=CYLINDRICAL_SURFACE('',#4027,0.4);
#3376=CYLINDRICAL_SURFACE('',#4033,0.685);
#3377=CYLINDRICAL_SURFACE('',#4034,0.4);
#3378=CYLINDRICAL_SURFACE('',#4036,0.8);
#3379=CYLINDRICAL_SURFACE('',#4039,0.685);
#3380=CYLINDRICAL_SURFACE('',#4042,0.165);
#3381=CYLINDRICAL_SURFACE('',#4046,0.165);
#3382=CYLINDRICAL_SURFACE('',#4050,0.925);
#3383=CYLINDRICAL_SURFACE('',#4054,0.6);
#3384=CYLINDRICAL_SURFACE('',#4058,2.5);
#3385=CYLINDRICAL_SURFACE('',#4062,4.);
#3386=CYLINDRICAL_SURFACE('',#4071,1.3);
#3387=CYLINDRICAL_SURFACE('',#4074,1.);
#3388=CYLINDRICAL_SURFACE('',#4078,0.2);
#3389=CYLINDRICAL_SURFACE('',#4081,0.6);
#3390=CYLINDRICAL_SURFACE('',#4090,0.4);
#3391=CYLINDRICAL_SURFACE('',#4098,0.4);
#3392=CYLINDRICAL_SURFACE('',#4099,0.15);
#3393=CYLINDRICAL_SURFACE('',#4101,0.15);
#3394=CYLINDRICAL_SURFACE('',#4103,0.4);
#3395=CYLINDRICAL_SURFACE('',#4114,0.16);
#3396=CYLINDRICAL_SURFACE('',#4117,2.2);
#3397=CYLINDRICAL_SURFACE('',#4123,0.275);
#3398=CYLINDRICAL_SURFACE('',#4126,0.275);
#3399=CYLINDRICAL_SURFACE('',#4129,0.275);
#3400=CYLINDRICAL_SURFACE('',#4132,0.275);
#3401=CYLINDRICAL_SURFACE('',#4135,0.275);
#3402=CYLINDRICAL_SURFACE('',#4138,0.275);
#3403=CYLINDRICAL_SURFACE('',#4141,0.16);
#3404=CYLINDRICAL_SURFACE('',#4144,4.);
#3405=CYLINDRICAL_SURFACE('',#4150,0.41);
#3406=CYLINDRICAL_SURFACE('',#4153,0.6);
#3407=CYLINDRICAL_SURFACE('',#4159,0.16);
#3408=CYLINDRICAL_SURFACE('',#4162,2.2);
#3409=CYLINDRICAL_SURFACE('',#4170,0.525);
#3410=CYLINDRICAL_SURFACE('',#4172,0.525);
#3411=CYLINDRICAL_SURFACE('',#4180,0.525);
#3412=CYLINDRICAL_SURFACE('',#4185,0.525);
#3413=CYLINDRICAL_SURFACE('',#4190,0.525);
#3414=CYLINDRICAL_SURFACE('',#4192,0.525);
#3415=CYLINDRICAL_SURFACE('',#4197,3.);
#3416=CYLINDRICAL_SURFACE('',#4206,0.275);
#3417=CYLINDRICAL_SURFACE('',#4209,0.275);
#3418=CYLINDRICAL_SURFACE('',#4212,0.275);
#3419=CYLINDRICAL_SURFACE('',#4215,0.275);
#3420=CYLINDRICAL_SURFACE('',#4218,0.275);
#3421=CYLINDRICAL_SURFACE('',#4221,0.275);
#3422=CYLINDRICAL_SURFACE('',#4224,0.34);
#3423=CYLINDRICAL_SURFACE('',#4227,2.5);
#3424=CYLINDRICAL_SURFACE('',#4232,4.);
#3425=CYLINDRICAL_SURFACE('',#4243,0.6);
#3426=CYLINDRICAL_SURFACE('',#4247,1.2);
#3427=CYLINDRICAL_SURFACE('',#4253,0.4);
#3428=CYLINDRICAL_SURFACE('',#4262,0.165);
#3429=CYLINDRICAL_SURFACE('',#4265,0.4);
#3430=CYLINDRICAL_SURFACE('',#4268,1.5);
#3431=CYLINDRICAL_SURFACE('',#4292,0.35);
#3432=CYLINDRICAL_SURFACE('',#4300,0.1954);
#3433=CYLINDRICAL_SURFACE('',#4324,0.685);
#3434=CYLINDRICAL_SURFACE('',#4330,0.685);
#3435=CYLINDRICAL_SURFACE('',#4336,0.46);
#3436=CYLINDRICAL_SURFACE('',#4342,0.425);
#3437=CYLINDRICAL_SURFACE('',#4350,0.24505);
#3438=CYLINDRICAL_SURFACE('',#4364,0.42);
#3439=CYLINDRICAL_SURFACE('',#4367,0.8);
#3440=CYLINDRICAL_SURFACE('',#4380,0.338975);
#3441=CYLINDRICAL_SURFACE('',#4400,0.1954);
#3442=ADVANCED_FACE('',(#495),#3364,.F.);
#3443=ADVANCED_FACE('',(#496),#3365,.F.);
#3444=ADVANCED_FACE('',(#497),#356,.T.);
#3445=ADVANCED_FACE('',(#498),#357,.T.);
#3446=ADVANCED_FACE('',(#499),#358,.T.);
#3447=ADVANCED_FACE('',(#500),#359,.T.);
#3448=ADVANCED_FACE('',(#501,#275,#276),#360,.T.);
#3449=ADVANCED_FACE('',(#502,#277,#278),#361,.F.);
#3450=ADVANCED_FACE('',(#503),#3366,.F.);
#3451=ADVANCED_FACE('',(#504),#362,.T.);
#3452=ADVANCED_FACE('',(#505),#363,.T.);
#3453=ADVANCED_FACE('',(#506),#364,.T.);
#3454=ADVANCED_FACE('',(#507),#365,.T.);
#3455=ADVANCED_FACE('',(#508,#279),#366,.T.);
#3456=ADVANCED_FACE('',(#509,#280),#367,.F.);
#3457=ADVANCED_FACE('',(#510),#3367,.F.);
#3458=ADVANCED_FACE('',(#511),#368,.T.);
#3459=ADVANCED_FACE('',(#512),#369,.T.);
#3460=ADVANCED_FACE('',(#513),#370,.T.);
#3461=ADVANCED_FACE('',(#514),#371,.T.);
#3462=ADVANCED_FACE('',(#515,#281),#372,.T.);
#3463=ADVANCED_FACE('',(#516,#282),#373,.F.);
#3464=ADVANCED_FACE('',(#517),#3368,.F.);
#3465=ADVANCED_FACE('',(#518),#374,.T.);
#3466=ADVANCED_FACE('',(#519),#3369,.F.);
#3467=ADVANCED_FACE('',(#520),#375,.T.);
#3468=ADVANCED_FACE('',(#521),#3370,.F.);
#3469=ADVANCED_FACE('',(#522),#376,.T.);
#3470=ADVANCED_FACE('',(#523),#3371,.F.);
#3471=ADVANCED_FACE('',(#524),#377,.T.);
#3472=ADVANCED_FACE('',(#525),#3372,.F.);
#3473=ADVANCED_FACE('',(#526),#378,.T.);
#3474=ADVANCED_FACE('',(#527),#3373,.F.);
#3475=ADVANCED_FACE('',(#528),#379,.T.);
#3476=ADVANCED_FACE('',(#529),#3374,.F.);
#3477=ADVANCED_FACE('',(#530),#3375,.F.);
#3478=ADVANCED_FACE('',(#531),#380,.T.);
#3479=ADVANCED_FACE('',(#532),#381,.T.);
#3480=ADVANCED_FACE('',(#533),#3376,.F.);
#3481=ADVANCED_FACE('',(#534),#3377,.F.);
#3482=ADVANCED_FACE('',(#535),#3378,.F.);
#3483=ADVANCED_FACE('',(#536),#3379,.F.);
#3484=ADVANCED_FACE('',(#537,#283),#382,.F.);
#3485=ADVANCED_FACE('',(#538),#3380,.F.);
#3486=ADVANCED_FACE('',(#539),#383,.F.);
#3487=ADVANCED_FACE('',(#540),#3381,.F.);
#3488=ADVANCED_FACE('',(#541),#384,.F.);
#3489=ADVANCED_FACE('',(#542),#3382,.F.);
#3490=ADVANCED_FACE('',(#543),#385,.F.);
#3491=ADVANCED_FACE('',(#544),#3383,.F.);
#3492=ADVANCED_FACE('',(#545,#284),#386,.F.);
#3493=ADVANCED_FACE('',(#546),#3384,.F.);
#3494=ADVANCED_FACE('',(#547,#285),#387,.T.);
#3495=ADVANCED_FACE('',(#548,#286),#3385,.T.);
#3496=ADVANCED_FACE('',(#549,#287,#288,#289,#290,#291,#292,#293),#388,.T.);
#3497=ADVANCED_FACE('',(#550,#294,#295,#296),#389,.F.);
#3498=ADVANCED_FACE('',(#551,#297),#390,.T.);
#3499=ADVANCED_FACE('',(#552),#3386,.T.);
#3500=ADVANCED_FACE('',(#553),#391,.F.);
#3501=ADVANCED_FACE('',(#554),#3387,.T.);
#3502=ADVANCED_FACE('',(#555),#392,.T.);
#3503=ADVANCED_FACE('',(#556),#3388,.F.);
#3504=ADVANCED_FACE('',(#557),#3389,.T.);
#3505=ADVANCED_FACE('',(#558,#298),#393,.T.);
#3506=ADVANCED_FACE('',(#559,#299),#394,.F.);
#3507=ADVANCED_FACE('',(#560,#300),#395,.F.);
#3508=ADVANCED_FACE('',(#561),#3390,.T.);
#3509=ADVANCED_FACE('',(#562,#301),#396,.T.);
#3510=ADVANCED_FACE('',(#563,#302),#397,.F.);
#3511=ADVANCED_FACE('',(#564),#3391,.T.);
#3512=ADVANCED_FACE('',(#565),#3392,.T.);
#3513=ADVANCED_FACE('',(#566),#3393,.T.);
#3514=ADVANCED_FACE('',(#567),#398,.T.);
#3515=ADVANCED_FACE('',(#568),#3394,.T.);
#3516=ADVANCED_FACE('',(#569,#303),#399,.T.);
#3517=ADVANCED_FACE('',(#570),#400,.F.);
#3518=ADVANCED_FACE('',(#571),#165,.T.);
#3519=ADVANCED_FACE('',(#572),#401,.T.);
#3520=ADVANCED_FACE('',(#573),#402,.F.);
#3521=ADVANCED_FACE('',(#574),#3395,.F.);
#3522=ADVANCED_FACE('',(#575),#3396,.T.);
#3523=ADVANCED_FACE('',(#576,#304),#403,.T.);
#3524=ADVANCED_FACE('',(#577,#305),#404,.F.);
#3525=ADVANCED_FACE('',(#578),#3397,.F.);
#3526=ADVANCED_FACE('',(#579),#3398,.F.);
#3527=ADVANCED_FACE('',(#580),#3399,.F.);
#3528=ADVANCED_FACE('',(#581),#3400,.F.);
#3529=ADVANCED_FACE('',(#582),#3401,.F.);
#3530=ADVANCED_FACE('',(#583),#3402,.F.);
#3531=ADVANCED_FACE('',(#584),#3403,.F.);
#3532=ADVANCED_FACE('',(#585),#3404,.T.);
#3533=ADVANCED_FACE('',(#586,#306,#307,#308,#309,#310,#311,#312),#405,.T.);
#3534=ADVANCED_FACE('',(#587,#313,#314,#315,#316,#317,#318,#319),#406,.F.);
#3535=ADVANCED_FACE('',(#588),#3405,.F.);
#3536=ADVANCED_FACE('',(#589),#3406,.T.);
#3537=ADVANCED_FACE('',(#590,#320),#407,.T.);
#3538=ADVANCED_FACE('',(#591,#321),#408,.T.);
#3539=ADVANCED_FACE('',(#592),#3407,.F.);
#3540=ADVANCED_FACE('',(#593),#3408,.T.);
#3541=ADVANCED_FACE('',(#594,#322),#409,.T.);
#3542=ADVANCED_FACE('',(#595,#323),#410,.F.);
#3543=ADVANCED_FACE('',(#596),#411,.F.);
#3544=ADVANCED_FACE('',(#597),#3409,.F.);
#3545=ADVANCED_FACE('',(#598),#3410,.F.);
#3546=ADVANCED_FACE('',(#599),#412,.F.);
#3547=ADVANCED_FACE('',(#600),#413,.F.);
#3548=ADVANCED_FACE('',(#601),#3411,.F.);
#3549=ADVANCED_FACE('',(#602),#414,.F.);
#3550=ADVANCED_FACE('',(#603),#3412,.F.);
#3551=ADVANCED_FACE('',(#604),#415,.F.);
#3552=ADVANCED_FACE('',(#605),#3413,.F.);
#3553=ADVANCED_FACE('',(#606),#3414,.F.);
#3554=ADVANCED_FACE('',(#607),#416,.F.);
#3555=ADVANCED_FACE('',(#608),#3415,.T.);
#3556=ADVANCED_FACE('',(#609),#3416,.F.);
#3557=ADVANCED_FACE('',(#610),#3417,.F.);
#3558=ADVANCED_FACE('',(#611),#3418,.F.);
#3559=ADVANCED_FACE('',(#612),#3419,.F.);
#3560=ADVANCED_FACE('',(#613),#3420,.F.);
#3561=ADVANCED_FACE('',(#614),#3421,.F.);
#3562=ADVANCED_FACE('',(#615),#3422,.F.);
#3563=ADVANCED_FACE('',(#616),#3423,.F.);
#3564=ADVANCED_FACE('',(#617,#324),#417,.F.);
#3565=ADVANCED_FACE('',(#618,#325),#418,.T.);
#3566=ADVANCED_FACE('',(#619),#3424,.T.);
#3567=ADVANCED_FACE('',(#620,#326,#327,#328,#329,#330,#331,#332),#419,.T.);
#3568=ADVANCED_FACE('',(#621,#333,#334,#335,#336,#337,#338,#339),#420,.F.);
#3569=ADVANCED_FACE('',(#622),#166,.T.);
#3570=ADVANCED_FACE('',(#623),#421,.T.);
#3571=ADVANCED_FACE('',(#624),#422,.F.);
#3572=ADVANCED_FACE('',(#625),#3425,.T.);
#3573=ADVANCED_FACE('',(#626),#423,.F.);
#3574=ADVANCED_FACE('',(#627),#3426,.T.);
#3575=ADVANCED_FACE('',(#628),#424,.T.);
#3576=ADVANCED_FACE('',(#629,#340),#425,.F.);
#3577=ADVANCED_FACE('',(#630),#3427,.T.);
#3578=ADVANCED_FACE('',(#631),#426,.T.);
#3579=ADVANCED_FACE('',(#632),#427,.F.);
#3580=ADVANCED_FACE('',(#633),#428,.T.);
#3581=ADVANCED_FACE('',(#634),#3428,.F.);
#3582=ADVANCED_FACE('',(#635),#429,.T.);
#3583=ADVANCED_FACE('',(#636,#341),#3429,.F.);
#3584=ADVANCED_FACE('',(#637,#342),#3430,.T.);
#3585=ADVANCED_FACE('',(#638,#343),#430,.T.);
#3586=ADVANCED_FACE('',(#639,#344),#431,.F.);
#3587=ADVANCED_FACE('',(#640),#432,.T.);
#3588=ADVANCED_FACE('',(#641),#433,.T.);
#3589=ADVANCED_FACE('',(#642),#434,.T.);
#3590=ADVANCED_FACE('',(#643),#435,.T.);
#3591=ADVANCED_FACE('',(#644),#436,.T.);
#3592=ADVANCED_FACE('',(#645),#437,.F.);
#3593=ADVANCED_FACE('',(#646),#438,.T.);
#3594=ADVANCED_FACE('',(#647),#439,.T.);
#3595=ADVANCED_FACE('',(#648),#440,.T.);
#3596=ADVANCED_FACE('',(#649),#441,.T.);
#3597=ADVANCED_FACE('',(#650),#442,.T.);
#3598=ADVANCED_FACE('',(#651),#443,.F.);
#3599=ADVANCED_FACE('',(#652),#444,.T.);
#3600=ADVANCED_FACE('',(#653),#149,.T.);
#3601=ADVANCED_FACE('',(#654),#3431,.T.);
#3602=ADVANCED_FACE('',(#655),#150,.T.);
#3603=ADVANCED_FACE('',(#656,#345),#445,.T.);
#3604=ADVANCED_FACE('',(#657),#151,.T.);
#3605=ADVANCED_FACE('',(#658),#3432,.T.);
#3606=ADVANCED_FACE('',(#659),#152,.T.);
#3607=ADVANCED_FACE('',(#660),#446,.T.);
#3608=ADVANCED_FACE('',(#661),#447,.F.);
#3609=ADVANCED_FACE('',(#662),#448,.F.);
#3610=ADVANCED_FACE('',(#663),#449,.F.);
#3611=ADVANCED_FACE('',(#664),#450,.F.);
#3612=ADVANCED_FACE('',(#665),#451,.F.);
#3613=ADVANCED_FACE('',(#666),#452,.F.);
#3614=ADVANCED_FACE('',(#667),#453,.F.);
#3615=ADVANCED_FACE('',(#668),#454,.F.);
#3616=ADVANCED_FACE('',(#669,#346),#455,.F.);
#3617=ADVANCED_FACE('',(#670,#347),#456,.T.);
#3618=ADVANCED_FACE('',(#671),#457,.T.);
#3619=ADVANCED_FACE('',(#672),#458,.T.);
#3620=ADVANCED_FACE('',(#673),#459,.T.);
#3621=ADVANCED_FACE('',(#674),#460,.T.);
#3622=ADVANCED_FACE('',(#675),#461,.T.);
#3623=ADVANCED_FACE('',(#676),#462,.T.);
#3624=ADVANCED_FACE('',(#677),#3433,.T.);
#3625=ADVANCED_FACE('',(#678,#348),#463,.T.);
#3626=ADVANCED_FACE('',(#679),#153,.T.);
#3627=ADVANCED_FACE('',(#680),#3434,.T.);
#3628=ADVANCED_FACE('',(#681),#154,.T.);
#3629=ADVANCED_FACE('',(#682,#349),#464,.T.);
#3630=ADVANCED_FACE('',(#683),#3435,.F.);
#3631=ADVANCED_FACE('',(#684),#465,.T.);
#3632=ADVANCED_FACE('',(#685),#155,.T.);
#3633=ADVANCED_FACE('',(#686),#3436,.T.);
#3634=ADVANCED_FACE('',(#687),#156,.T.);
#3635=ADVANCED_FACE('',(#688,#350),#466,.T.);
#3636=ADVANCED_FACE('',(#689),#157,.T.);
#3637=ADVANCED_FACE('',(#690),#3437,.T.);
#3638=ADVANCED_FACE('',(#691),#158,.T.);
#3639=ADVANCED_FACE('',(#692),#467,.T.);
#3640=ADVANCED_FACE('',(#693),#468,.F.);
#3641=ADVANCED_FACE('',(#694),#469,.F.);
#3642=ADVANCED_FACE('',(#695),#470,.F.);
#3643=ADVANCED_FACE('',(#696),#471,.F.);
#3644=ADVANCED_FACE('',(#697),#472,.F.);
#3645=ADVANCED_FACE('',(#698),#473,.F.);
#3646=ADVANCED_FACE('',(#699),#474,.F.);
#3647=ADVANCED_FACE('',(#700),#475,.F.);
#3648=ADVANCED_FACE('',(#701),#3438,.F.);
#3649=ADVANCED_FACE('',(#702),#3439,.T.);
#3650=ADVANCED_FACE('',(#703,#351),#476,.T.);
#3651=ADVANCED_FACE('',(#704,#352),#477,.F.);
#3652=ADVANCED_FACE('',(#705),#159,.T.);
#3653=ADVANCED_FACE('',(#706),#160,.T.);
#3654=ADVANCED_FACE('',(#707),#478,.T.);
#3655=ADVANCED_FACE('',(#708),#479,.T.);
#3656=ADVANCED_FACE('',(#709),#480,.T.);
#3657=ADVANCED_FACE('',(#710),#3440,.F.);
#3658=ADVANCED_FACE('',(#711),#481,.T.);
#3659=ADVANCED_FACE('',(#712),#482,.T.);
#3660=ADVANCED_FACE('',(#713),#483,.T.);
#3661=ADVANCED_FACE('',(#714,#353),#484,.T.);
#3662=ADVANCED_FACE('',(#715,#354),#485,.F.);
#3663=ADVANCED_FACE('',(#716),#486,.F.);
#3664=ADVANCED_FACE('',(#717),#487,.F.);
#3665=ADVANCED_FACE('',(#718),#488,.F.);
#3666=ADVANCED_FACE('',(#719),#489,.F.);
#3667=ADVANCED_FACE('',(#720),#490,.F.);
#3668=ADVANCED_FACE('',(#721),#491,.F.);
#3669=ADVANCED_FACE('',(#722),#492,.F.);
#3670=ADVANCED_FACE('',(#723,#355),#493,.T.);
#3671=ADVANCED_FACE('',(#724),#161,.T.);
#3672=ADVANCED_FACE('',(#725),#3441,.T.);
#3673=ADVANCED_FACE('',(#726),#162,.T.);
#3674=ADVANCED_FACE('',(#727),#494,.T.);
#3675=CLOSED_SHELL('',(#3442,#3443,#3444,#3445,#3446,#3447,#3448,#3449));
#3676=CLOSED_SHELL('',(#3450,#3451,#3452,#3453,#3454,#3455,#3456));
#3677=CLOSED_SHELL('',(#3457,#3458,#3459,#3460,#3461,#3462,#3463));
#3678=CLOSED_SHELL('',(#3464,#3465,#3466,#3467,#3468,#3469,#3470,#3471,
#3472,#3473,#3474,#3475,#3476,#3477,#3478,#3479,#3480,#3481,#3482,#3483,
#3484,#3485,#3486,#3487,#3488,#3489,#3490,#3491,#3492,#3493,#3494,#3495,
#3496,#3497));
#3679=CLOSED_SHELL('',(#3498,#3499,#3500,#3501,#3502));
#3680=CLOSED_SHELL('',(#3503,#3504,#3505,#3506));
#3681=CLOSED_SHELL('',(#3507,#3508,#3509,#3510,#3511,#3512,#3513,#3514,
#3515,#3516,#3517));
#3682=CLOSED_SHELL('',(#3518,#3519,#3520));
#3683=CLOSED_SHELL('',(#3521,#3522,#3523,#3524));
#3684=CLOSED_SHELL('',(#3525,#3526,#3527,#3528,#3529,#3530,#3531,#3532,
#3533,#3534));
#3685=CLOSED_SHELL('',(#3535,#3536,#3537,#3538,#3539,#3540,#3541,#3542));
#3686=CLOSED_SHELL('',(#3543,#3544,#3545,#3546,#3547,#3548,#3549,#3550,
#3551,#3552,#3553,#3554,#3555,#3556,#3557,#3558,#3559,#3560,#3561,#3562,
#3563,#3564,#3565,#3566,#3567,#3568));
#3687=CLOSED_SHELL('',(#3569,#3570,#3571));
#3688=CLOSED_SHELL('',(#3572,#3573,#3574,#3575,#3576));
#3689=CLOSED_SHELL('',(#3577,#3578,#3579));
#3690=CLOSED_SHELL('',(#3580,#3581,#3582,#3583,#3584,#3585,#3586));
#3691=CLOSED_SHELL('',(#3587,#3588,#3589,#3590,#3591,#3592));
#3692=CLOSED_SHELL('',(#3593,#3594,#3595,#3596,#3597,#3598));
#3693=CLOSED_SHELL('',(#3599,#3600,#3601,#3602,#3603,#3604,#3605,#3606,
#3607));
#3694=CLOSED_SHELL('',(#3608,#3609,#3610,#3611,#3612,#3613,#3614,#3615));
#3695=CLOSED_SHELL('',(#3616,#3617,#3618,#3619,#3620,#3621,#3622,#3623,
#3624,#3625,#3626,#3627,#3628,#3629,#3630));
#3696=CLOSED_SHELL('',(#3631,#3632,#3633,#3634,#3635,#3636,#3637,#3638,
#3639));
#3697=CLOSED_SHELL('',(#3640,#3641,#3642,#3643,#3644,#3645,#3646,#3647));
#3698=CLOSED_SHELL('',(#3648,#3649,#3650,#3651));
#3699=CLOSED_SHELL('',(#3652,#3653,#3654,#3655,#3656,#3657,#3658,#3659,
#3660,#3661,#3662));
#3700=CLOSED_SHELL('',(#3663,#3664,#3665,#3666,#3667,#3668,#3669,#3670,
#3671,#3672,#3673,#3674));
#3701=DERIVED_UNIT_ELEMENT(#3749,1.);
#3702=DERIVED_UNIT_ELEMENT(#8430,-3.);
#3703=DERIVED_UNIT_ELEMENT(#3749,1.);
#3704=DERIVED_UNIT_ELEMENT(#8430,-3.);
#3705=DERIVED_UNIT_ELEMENT(#3749,1.);
#3706=DERIVED_UNIT_ELEMENT(#8430,-3.);
#3707=DERIVED_UNIT_ELEMENT(#3749,1.);
#3708=DERIVED_UNIT_ELEMENT(#8430,-3.);
#3709=DERIVED_UNIT_ELEMENT(#3749,1.);
#3710=DERIVED_UNIT_ELEMENT(#8430,-3.);
#3711=DERIVED_UNIT_ELEMENT(#3749,1.);
#3712=DERIVED_UNIT_ELEMENT(#8430,-3.);
#3713=DERIVED_UNIT_ELEMENT(#3749,1.);
#3714=DERIVED_UNIT_ELEMENT(#8430,-3.);
#3715=DERIVED_UNIT_ELEMENT(#3749,1.);
#3716=DERIVED_UNIT_ELEMENT(#8430,-3.);
#3717=DERIVED_UNIT_ELEMENT(#3749,1.);
#3718=DERIVED_UNIT_ELEMENT(#8430,-3.);
#3719=DERIVED_UNIT_ELEMENT(#3749,1.);
#3720=DERIVED_UNIT_ELEMENT(#8430,-3.);
#3721=DERIVED_UNIT_ELEMENT(#3749,1.);
#3722=DERIVED_UNIT_ELEMENT(#8430,-3.);
#3723=DERIVED_UNIT_ELEMENT(#3749,1.);
#3724=DERIVED_UNIT_ELEMENT(#8430,-3.);
#3725=DERIVED_UNIT_ELEMENT(#3749,1.);
#3726=DERIVED_UNIT_ELEMENT(#8430,-3.);
#3727=DERIVED_UNIT_ELEMENT(#3749,1.);
#3728=DERIVED_UNIT_ELEMENT(#8430,-3.);
#3729=DERIVED_UNIT_ELEMENT(#3749,1.);
#3730=DERIVED_UNIT_ELEMENT(#8430,-3.);
#3731=DERIVED_UNIT_ELEMENT(#3749,1.);
#3732=DERIVED_UNIT_ELEMENT(#8430,-3.);
#3733=DERIVED_UNIT_ELEMENT(#3749,1.);
#3734=DERIVED_UNIT_ELEMENT(#8430,-3.);
#3735=DERIVED_UNIT_ELEMENT(#3749,1.);
#3736=DERIVED_UNIT_ELEMENT(#8430,-3.);
#3737=DERIVED_UNIT_ELEMENT(#3749,1.);
#3738=DERIVED_UNIT_ELEMENT(#8430,-3.);
#3739=DERIVED_UNIT_ELEMENT(#3749,1.);
#3740=DERIVED_UNIT_ELEMENT(#8430,-3.);
#3741=DERIVED_UNIT_ELEMENT(#3749,1.);
#3742=DERIVED_UNIT_ELEMENT(#8430,-3.);
#3743=DERIVED_UNIT_ELEMENT(#3749,1.);
#3744=DERIVED_UNIT_ELEMENT(#8430,-3.);
#3745=DERIVED_UNIT_ELEMENT(#3749,1.);
#3746=DERIVED_UNIT_ELEMENT(#8430,-3.);
#3747=DERIVED_UNIT_ELEMENT(#3749,1.);
#3748=DERIVED_UNIT_ELEMENT(#8430,-3.);
#3749=(
MASS_UNIT()
NAMED_UNIT(*)
SI_UNIT(.KILO.,.GRAM.)
);
#3750=DERIVED_UNIT((#3701,#3702));
#3751=DERIVED_UNIT((#3703,#3704));
#3752=DERIVED_UNIT((#3705,#3706));
#3753=DERIVED_UNIT((#3707,#3708));
#3754=DERIVED_UNIT((#3709,#3710));
#3755=DERIVED_UNIT((#3711,#3712));
#3756=DERIVED_UNIT((#3713,#3714));
#3757=DERIVED_UNIT((#3715,#3716));
#3758=DERIVED_UNIT((#3717,#3718));
#3759=DERIVED_UNIT((#3719,#3720));
#3760=DERIVED_UNIT((#3721,#3722));
#3761=DERIVED_UNIT((#3723,#3724));
#3762=DERIVED_UNIT((#3725,#3726));
#3763=DERIVED_UNIT((#3727,#3728));
#3764=DERIVED_UNIT((#3729,#3730));
#3765=DERIVED_UNIT((#3731,#3732));
#3766=DERIVED_UNIT((#3733,#3734));
#3767=DERIVED_UNIT((#3735,#3736));
#3768=DERIVED_UNIT((#3737,#3738));
#3769=DERIVED_UNIT((#3739,#3740));
#3770=DERIVED_UNIT((#3741,#3742));
#3771=DERIVED_UNIT((#3743,#3744));
#3772=DERIVED_UNIT((#3745,#3746));
#3773=DERIVED_UNIT((#3747,#3748));
#3774=MEASURE_REPRESENTATION_ITEM('density measure',
POSITIVE_RATIO_MEASURE(7850.),#3750);
#3775=MEASURE_REPRESENTATION_ITEM('density measure',
POSITIVE_RATIO_MEASURE(7850.),#3751);
#3776=MEASURE_REPRESENTATION_ITEM('density measure',
POSITIVE_RATIO_MEASURE(7850.),#3752);
#3777=MEASURE_REPRESENTATION_ITEM('density measure',
POSITIVE_RATIO_MEASURE(7850.),#3753);
#3778=MEASURE_REPRESENTATION_ITEM('density measure',
POSITIVE_RATIO_MEASURE(7850.),#3754);
#3779=MEASURE_REPRESENTATION_ITEM('density measure',
POSITIVE_RATIO_MEASURE(7850.),#3755);
#3780=MEASURE_REPRESENTATION_ITEM('density measure',
POSITIVE_RATIO_MEASURE(7850.),#3756);
#3781=MEASURE_REPRESENTATION_ITEM('density measure',
POSITIVE_RATIO_MEASURE(7850.),#3757);
#3782=MEASURE_REPRESENTATION_ITEM('density measure',
POSITIVE_RATIO_MEASURE(7850.),#3758);
#3783=MEASURE_REPRESENTATION_ITEM('density measure',
POSITIVE_RATIO_MEASURE(7850.),#3759);
#3784=MEASURE_REPRESENTATION_ITEM('density measure',
POSITIVE_RATIO_MEASURE(7850.),#3760);
#3785=MEASURE_REPRESENTATION_ITEM('density measure',
POSITIVE_RATIO_MEASURE(7850.),#3761);
#3786=MEASURE_REPRESENTATION_ITEM('density measure',
POSITIVE_RATIO_MEASURE(7850.),#3762);
#3787=MEASURE_REPRESENTATION_ITEM('density measure',
POSITIVE_RATIO_MEASURE(7850.),#3763);
#3788=MEASURE_REPRESENTATION_ITEM('density measure',
POSITIVE_RATIO_MEASURE(7850.),#3764);
#3789=MEASURE_REPRESENTATION_ITEM('density measure',
POSITIVE_RATIO_MEASURE(7850.),#3765);
#3790=MEASURE_REPRESENTATION_ITEM('density measure',
POSITIVE_RATIO_MEASURE(7850.),#3766);
#3791=MEASURE_REPRESENTATION_ITEM('density measure',
POSITIVE_RATIO_MEASURE(7850.),#3767);
#3792=MEASURE_REPRESENTATION_ITEM('density measure',
POSITIVE_RATIO_MEASURE(7850.),#3768);
#3793=MEASURE_REPRESENTATION_ITEM('density measure',
POSITIVE_RATIO_MEASURE(7850.),#3769);
#3794=MEASURE_REPRESENTATION_ITEM('density measure',
POSITIVE_RATIO_MEASURE(7850.),#3770);
#3795=MEASURE_REPRESENTATION_ITEM('density measure',
POSITIVE_RATIO_MEASURE(7850.),#3771);
#3796=MEASURE_REPRESENTATION_ITEM('density measure',
POSITIVE_RATIO_MEASURE(7850.),#3772);
#3797=MEASURE_REPRESENTATION_ITEM('density measure',
POSITIVE_RATIO_MEASURE(7850.),#3773);
#3798=PROPERTY_DEFINITION_REPRESENTATION(#3918,#3846);
#3799=PROPERTY_DEFINITION_REPRESENTATION(#3919,#3847);
#3800=PROPERTY_DEFINITION_REPRESENTATION(#3920,#3848);
#3801=PROPERTY_DEFINITION_REPRESENTATION(#3921,#3849);
#3802=PROPERTY_DEFINITION_REPRESENTATION(#3922,#3850);
#3803=PROPERTY_DEFINITION_REPRESENTATION(#3923,#3851);
#3804=PROPERTY_DEFINITION_REPRESENTATION(#3924,#3852);
#3805=PROPERTY_DEFINITION_REPRESENTATION(#3925,#3853);
#3806=PROPERTY_DEFINITION_REPRESENTATION(#3926,#3854);
#3807=PROPERTY_DEFINITION_REPRESENTATION(#3927,#3855);
#3808=PROPERTY_DEFINITION_REPRESENTATION(#3928,#3856);
#3809=PROPERTY_DEFINITION_REPRESENTATION(#3929,#3857);
#3810=PROPERTY_DEFINITION_REPRESENTATION(#3930,#3858);
#3811=PROPERTY_DEFINITION_REPRESENTATION(#3931,#3859);
#3812=PROPERTY_DEFINITION_REPRESENTATION(#3932,#3860);
#3813=PROPERTY_DEFINITION_REPRESENTATION(#3933,#3861);
#3814=PROPERTY_DEFINITION_REPRESENTATION(#3934,#3862);
#3815=PROPERTY_DEFINITION_REPRESENTATION(#3935,#3863);
#3816=PROPERTY_DEFINITION_REPRESENTATION(#3936,#3864);
#3817=PROPERTY_DEFINITION_REPRESENTATION(#3937,#3865);
#3818=PROPERTY_DEFINITION_REPRESENTATION(#3938,#3866);
#3819=PROPERTY_DEFINITION_REPRESENTATION(#3939,#3867);
#3820=PROPERTY_DEFINITION_REPRESENTATION(#3940,#3868);
#3821=PROPERTY_DEFINITION_REPRESENTATION(#3941,#3869);
#3822=PROPERTY_DEFINITION_REPRESENTATION(#3942,#3870);
#3823=PROPERTY_DEFINITION_REPRESENTATION(#3943,#3871);
#3824=PROPERTY_DEFINITION_REPRESENTATION(#3944,#3872);
#3825=PROPERTY_DEFINITION_REPRESENTATION(#3945,#3873);
#3826=PROPERTY_DEFINITION_REPRESENTATION(#3946,#3874);
#3827=PROPERTY_DEFINITION_REPRESENTATION(#3947,#3875);
#3828=PROPERTY_DEFINITION_REPRESENTATION(#3948,#3876);
#3829=PROPERTY_DEFINITION_REPRESENTATION(#3949,#3877);
#3830=PROPERTY_DEFINITION_REPRESENTATION(#3950,#3878);
#3831=PROPERTY_DEFINITION_REPRESENTATION(#3951,#3879);
#3832=PROPERTY_DEFINITION_REPRESENTATION(#3952,#3880);
#3833=PROPERTY_DEFINITION_REPRESENTATION(#3953,#3881);
#3834=PROPERTY_DEFINITION_REPRESENTATION(#3954,#3882);
#3835=PROPERTY_DEFINITION_REPRESENTATION(#3955,#3883);
#3836=PROPERTY_DEFINITION_REPRESENTATION(#3956,#3884);
#3837=PROPERTY_DEFINITION_REPRESENTATION(#3957,#3885);
#3838=PROPERTY_DEFINITION_REPRESENTATION(#3958,#3886);
#3839=PROPERTY_DEFINITION_REPRESENTATION(#3959,#3887);
#3840=PROPERTY_DEFINITION_REPRESENTATION(#3960,#3888);
#3841=PROPERTY_DEFINITION_REPRESENTATION(#3961,#3889);
#3842=PROPERTY_DEFINITION_REPRESENTATION(#3962,#3890);
#3843=PROPERTY_DEFINITION_REPRESENTATION(#3963,#3891);
#3844=PROPERTY_DEFINITION_REPRESENTATION(#3964,#3892);
#3845=PROPERTY_DEFINITION_REPRESENTATION(#3965,#3893);
#3846=REPRESENTATION('material name',(#3894),#8404);
#3847=REPRESENTATION('density',(#3774),#8404);
#3848=REPRESENTATION('material name',(#3895),#8405);
#3849=REPRESENTATION('density',(#3775),#8405);
#3850=REPRESENTATION('material name',(#3896),#8406);
#3851=REPRESENTATION('density',(#3776),#8406);
#3852=REPRESENTATION('material name',(#3897),#8407);
#3853=REPRESENTATION('density',(#3777),#8407);
#3854=REPRESENTATION('material name',(#3898),#8408);
#3855=REPRESENTATION('density',(#3778),#8408);
#3856=REPRESENTATION('material name',(#3899),#8409);
#3857=REPRESENTATION('density',(#3779),#8409);
#3858=REPRESENTATION('material name',(#3900),#8410);
#3859=REPRESENTATION('density',(#3780),#8410);
#3860=REPRESENTATION('material name',(#3901),#8411);
#3861=REPRESENTATION('density',(#3781),#8411);
#3862=REPRESENTATION('material name',(#3902),#8412);
#3863=REPRESENTATION('density',(#3782),#8412);
#3864=REPRESENTATION('material name',(#3903),#8413);
#3865=REPRESENTATION('density',(#3783),#8413);
#3866=REPRESENTATION('material name',(#3904),#8414);
#3867=REPRESENTATION('density',(#3784),#8414);
#3868=REPRESENTATION('material name',(#3905),#8415);
#3869=REPRESENTATION('density',(#3785),#8415);
#3870=REPRESENTATION('material name',(#3906),#8416);
#3871=REPRESENTATION('density',(#3786),#8416);
#3872=REPRESENTATION('material name',(#3907),#8417);
#3873=REPRESENTATION('density',(#3787),#8417);
#3874=REPRESENTATION('material name',(#3908),#8418);
#3875=REPRESENTATION('density',(#3788),#8418);
#3876=REPRESENTATION('material name',(#3909),#8419);
#3877=REPRESENTATION('density',(#3789),#8419);
#3878=REPRESENTATION('material name',(#3910),#8420);
#3879=REPRESENTATION('density',(#3790),#8420);
#3880=REPRESENTATION('material name',(#3911),#8421);
#3881=REPRESENTATION('density',(#3791),#8421);
#3882=REPRESENTATION('material name',(#3912),#8422);
#3883=REPRESENTATION('density',(#3792),#8422);
#3884=REPRESENTATION('material name',(#3913),#8423);
#3885=REPRESENTATION('density',(#3793),#8423);
#3886=REPRESENTATION('material name',(#3914),#8424);
#3887=REPRESENTATION('density',(#3794),#8424);
#3888=REPRESENTATION('material name',(#3915),#8425);
#3889=REPRESENTATION('density',(#3795),#8425);
#3890=REPRESENTATION('material name',(#3916),#8426);
#3891=REPRESENTATION('density',(#3796),#8426);
#3892=REPRESENTATION('material name',(#3917),#8427);
#3893=REPRESENTATION('density',(#3797),#8427);
#3894=DESCRIPTIVE_REPRESENTATION_ITEM('Steel','Steel');
#3895=DESCRIPTIVE_REPRESENTATION_ITEM('Steel','Steel');
#3896=DESCRIPTIVE_REPRESENTATION_ITEM('Steel','Steel');
#3897=DESCRIPTIVE_REPRESENTATION_ITEM('Steel','Steel');
#3898=DESCRIPTIVE_REPRESENTATION_ITEM('Steel','Steel');
#3899=DESCRIPTIVE_REPRESENTATION_ITEM('Steel','Steel');
#3900=DESCRIPTIVE_REPRESENTATION_ITEM('Steel','Steel');
#3901=DESCRIPTIVE_REPRESENTATION_ITEM('Steel','Steel');
#3902=DESCRIPTIVE_REPRESENTATION_ITEM('Steel','Steel');
#3903=DESCRIPTIVE_REPRESENTATION_ITEM('Steel','Steel');
#3904=DESCRIPTIVE_REPRESENTATION_ITEM('Steel','Steel');
#3905=DESCRIPTIVE_REPRESENTATION_ITEM('Steel','Steel');
#3906=DESCRIPTIVE_REPRESENTATION_ITEM('Steel','Steel');
#3907=DESCRIPTIVE_REPRESENTATION_ITEM('Steel','Steel');
#3908=DESCRIPTIVE_REPRESENTATION_ITEM('Steel','Steel');
#3909=DESCRIPTIVE_REPRESENTATION_ITEM('Steel','Steel');
#3910=DESCRIPTIVE_REPRESENTATION_ITEM('Steel','Steel');
#3911=DESCRIPTIVE_REPRESENTATION_ITEM('Steel','Steel');
#3912=DESCRIPTIVE_REPRESENTATION_ITEM('Steel','Steel');
#3913=DESCRIPTIVE_REPRESENTATION_ITEM('Steel','Steel');
#3914=DESCRIPTIVE_REPRESENTATION_ITEM('Steel','Steel');
#3915=DESCRIPTIVE_REPRESENTATION_ITEM('Steel','Steel');
#3916=DESCRIPTIVE_REPRESENTATION_ITEM('Steel','Steel');
#3917=DESCRIPTIVE_REPRESENTATION_ITEM('Steel','Steel');
#3918=PROPERTY_DEFINITION('material property','material name',#8541);
#3919=PROPERTY_DEFINITION('material property','density of part',#8541);
#3920=PROPERTY_DEFINITION('material property','material name',#8542);
#3921=PROPERTY_DEFINITION('material property','density of part',#8542);
#3922=PROPERTY_DEFINITION('material property','material name',#8543);
#3923=PROPERTY_DEFINITION('material property','density of part',#8543);
#3924=PROPERTY_DEFINITION('material property','material name',#8544);
#3925=PROPERTY_DEFINITION('material property','density of part',#8544);
#3926=PROPERTY_DEFINITION('material property','material name',#8545);
#3927=PROPERTY_DEFINITION('material property','density of part',#8545);
#3928=PROPERTY_DEFINITION('material property','material name',#8546);
#3929=PROPERTY_DEFINITION('material property','density of part',#8546);
#3930=PROPERTY_DEFINITION('material property','material name',#8547);
#3931=PROPERTY_DEFINITION('material property','density of part',#8547);
#3932=PROPERTY_DEFINITION('material property','material name',#8548);
#3933=PROPERTY_DEFINITION('material property','density of part',#8548);
#3934=PROPERTY_DEFINITION('material property','material name',#8549);
#3935=PROPERTY_DEFINITION('material property','density of part',#8549);
#3936=PROPERTY_DEFINITION('material property','material name',#8550);
#3937=PROPERTY_DEFINITION('material property','density of part',#8550);
#3938=PROPERTY_DEFINITION('material property','material name',#8551);
#3939=PROPERTY_DEFINITION('material property','density of part',#8551);
#3940=PROPERTY_DEFINITION('material property','material name',#8552);
#3941=PROPERTY_DEFINITION('material property','density of part',#8552);
#3942=PROPERTY_DEFINITION('material property','material name',#8553);
#3943=PROPERTY_DEFINITION('material property','density of part',#8553);
#3944=PROPERTY_DEFINITION('material property','material name',#8554);
#3945=PROPERTY_DEFINITION('material property','density of part',#8554);
#3946=PROPERTY_DEFINITION('material property','material name',#8555);
#3947=PROPERTY_DEFINITION('material property','density of part',#8555);
#3948=PROPERTY_DEFINITION('material property','material name',#8556);
#3949=PROPERTY_DEFINITION('material property','density of part',#8556);
#3950=PROPERTY_DEFINITION('material property','material name',#8557);
#3951=PROPERTY_DEFINITION('material property','density of part',#8557);
#3952=PROPERTY_DEFINITION('material property','material name',#8558);
#3953=PROPERTY_DEFINITION('material property','density of part',#8558);
#3954=PROPERTY_DEFINITION('material property','material name',#8559);
#3955=PROPERTY_DEFINITION('material property','density of part',#8559);
#3956=PROPERTY_DEFINITION('material property','material name',#8560);
#3957=PROPERTY_DEFINITION('material property','density of part',#8560);
#3958=PROPERTY_DEFINITION('material property','material name',#8561);
#3959=PROPERTY_DEFINITION('material property','density of part',#8561);
#3960=PROPERTY_DEFINITION('material property','material name',#8562);
#3961=PROPERTY_DEFINITION('material property','density of part',#8562);
#3962=PROPERTY_DEFINITION('material property','material name',#8563);
#3963=PROPERTY_DEFINITION('material property','density of part',#8563);
#3964=PROPERTY_DEFINITION('material property','material name',#8564);
#3965=PROPERTY_DEFINITION('material property','density of part',#8564);
#3966=AXIS2_PLACEMENT_3D('',#5620,#4436,#4437);
#3967=AXIS2_PLACEMENT_3D('',#5621,#4438,#4439);
#3968=AXIS2_PLACEMENT_3D('',#5622,#4440,#4441);
#3969=AXIS2_PLACEMENT_3D('',#5624,#4442,#4443);
#3970=AXIS2_PLACEMENT_3D('',#5627,#4445,#4446);
#3971=AXIS2_PLACEMENT_3D('',#5628,#4447,#4448);
#3972=AXIS2_PLACEMENT_3D('',#5630,#4449,#4450);
#3973=AXIS2_PLACEMENT_3D('',#5633,#4452,#4453);
#3974=AXIS2_PLACEMENT_3D('',#5634,#4454,#4455);
#3975=AXIS2_PLACEMENT_3D('',#5643,#4460,#4461);
#3976=AXIS2_PLACEMENT_3D('',#5649,#4465,#4466);
#3977=AXIS2_PLACEMENT_3D('',#5655,#4470,#4471);
#3978=AXIS2_PLACEMENT_3D('',#5658,#4474,#4475);
#3979=AXIS2_PLACEMENT_3D('',#5659,#4476,#4477);
#3980=AXIS2_PLACEMENT_3D('',#5660,#4478,#4479);
#3981=AXIS2_PLACEMENT_3D('',#5661,#4480,#4481);
#3982=AXIS2_PLACEMENT_3D('',#5663,#4482,#4483);
#3983=AXIS2_PLACEMENT_3D('',#5666,#4485,#4486);
#3984=AXIS2_PLACEMENT_3D('',#5667,#4487,#4488);
#3985=AXIS2_PLACEMENT_3D('',#5676,#4493,#4494);
#3986=AXIS2_PLACEMENT_3D('',#5682,#4498,#4499);
#3987=AXIS2_PLACEMENT_3D('',#5688,#4503,#4504);
#3988=AXIS2_PLACEMENT_3D('',#5691,#4507,#4508);
#3989=AXIS2_PLACEMENT_3D('',#5692,#4509,#4510);
#3990=AXIS2_PLACEMENT_3D('',#5693,#4511,#4512);
#3991=AXIS2_PLACEMENT_3D('',#5694,#4513,#4514);
#3992=AXIS2_PLACEMENT_3D('',#5696,#4515,#4516);
#3993=AXIS2_PLACEMENT_3D('',#5699,#4518,#4519);
#3994=AXIS2_PLACEMENT_3D('',#5700,#4520,#4521);
#3995=AXIS2_PLACEMENT_3D('',#5709,#4526,#4527);
#3996=AXIS2_PLACEMENT_3D('',#5715,#4531,#4532);
#3997=AXIS2_PLACEMENT_3D('',#5721,#4536,#4537);
#3998=AXIS2_PLACEMENT_3D('',#5724,#4540,#4541);
#3999=AXIS2_PLACEMENT_3D('',#5725,#4542,#4543);
#4000=AXIS2_PLACEMENT_3D('',#5726,#4544,#4545);
#4001=AXIS2_PLACEMENT_3D('',#5727,#4546,#4547);
#4002=AXIS2_PLACEMENT_3D('',#5729,#4548,#4549);
#4003=AXIS2_PLACEMENT_3D('',#5732,#4551,#4552);
#4004=AXIS2_PLACEMENT_3D('',#5733,#4553,#4554);
#4005=AXIS2_PLACEMENT_3D('',#5734,#4555,#4556);
#4006=AXIS2_PLACEMENT_3D('',#5736,#4557,#4558);
#4007=AXIS2_PLACEMENT_3D('',#5739,#4560,#4561);
#4008=AXIS2_PLACEMENT_3D('',#5740,#4562,#4563);
#4009=AXIS2_PLACEMENT_3D('',#5741,#4564,#4565);
#4010=AXIS2_PLACEMENT_3D('',#5743,#4566,#4567);
#4011=AXIS2_PLACEMENT_3D('',#5746,#4569,#4570);
#4012=AXIS2_PLACEMENT_3D('',#5747,#4571,#4572);
#4013=AXIS2_PLACEMENT_3D('',#5748,#4573,#4574);
#4014=AXIS2_PLACEMENT_3D('',#5750,#4575,#4576);
#4015=AXIS2_PLACEMENT_3D('',#5753,#4578,#4579);
#4016=AXIS2_PLACEMENT_3D('',#5754,#4580,#4581);
#4017=AXIS2_PLACEMENT_3D('',#5755,#4582,#4583);
#4018=AXIS2_PLACEMENT_3D('',#5757,#4584,#4585);
#4019=AXIS2_PLACEMENT_3D('',#5760,#4587,#4588);
#4020=AXIS2_PLACEMENT_3D('',#5761,#4589,#4590);
#4021=AXIS2_PLACEMENT_3D('',#5762,#4591,#4592);
#4022=AXIS2_PLACEMENT_3D('',#5764,#4593,#4594);
#4023=AXIS2_PLACEMENT_3D('',#5767,#4596,#4597);
#4024=AXIS2_PLACEMENT_3D('',#5768,#4598,#4599);
#4025=AXIS2_PLACEMENT_3D('',#5769,#4600,#4601);
#4026=AXIS2_PLACEMENT_3D('',#5772,#4602,#4603);
#4027=AXIS2_PLACEMENT_3D('',#5791,#4604,#4605);
#4028=AXIS2_PLACEMENT_3D('',#5792,#4606,#4607);
#4029=AXIS2_PLACEMENT_3D('',#5812,#4608,#4609);
#4030=AXIS2_PLACEMENT_3D('',#5816,#4611,#4612);
#4031=AXIS2_PLACEMENT_3D('',#5818,#4614,#4615);
#4032=AXIS2_PLACEMENT_3D('',#5820,#4617,#4618);
#4033=AXIS2_PLACEMENT_3D('',#5822,#4620,#4621);
#4034=AXIS2_PLACEMENT_3D('',#5862,#4623,#4624);
#4035=AXIS2_PLACEMENT_3D('',#5864,#4625,#4626);
#4036=AXIS2_PLACEMENT_3D('',#5908,#4630,#4631);
#4037=AXIS2_PLACEMENT_3D('',#5909,#4632,#4633);
#4038=AXIS2_PLACEMENT_3D('',#5912,#4635,#4636);
#4039=AXIS2_PLACEMENT_3D('',#5913,#4637,#4638);
#4040=AXIS2_PLACEMENT_3D('',#5957,#4640,#4641);
#4041=AXIS2_PLACEMENT_3D('',#5958,#4642,#4643);
#4042=AXIS2_PLACEMENT_3D('',#5959,#4644,#4645);
#4043=AXIS2_PLACEMENT_3D('',#5961,#4646,#4647);
#4044=AXIS2_PLACEMENT_3D('',#5964,#4649,#4650);
#4045=AXIS2_PLACEMENT_3D('',#5965,#4651,#4652);
#4046=AXIS2_PLACEMENT_3D('',#5966,#4653,#4654);
#4047=AXIS2_PLACEMENT_3D('',#5968,#4655,#4656);
#4048=AXIS2_PLACEMENT_3D('',#5971,#4658,#4659);
#4049=AXIS2_PLACEMENT_3D('',#5972,#4660,#4661);
#4050=AXIS2_PLACEMENT_3D('',#5973,#4662,#4663);
#4051=AXIS2_PLACEMENT_3D('',#5975,#4664,#4665);
#4052=AXIS2_PLACEMENT_3D('',#5977,#4667,#4668);
#4053=AXIS2_PLACEMENT_3D('',#5978,#4669,#4670);
#4054=AXIS2_PLACEMENT_3D('',#5979,#4671,#4672);
#4055=AXIS2_PLACEMENT_3D('',#5981,#4673,#4674);
#4056=AXIS2_PLACEMENT_3D('',#5984,#4676,#4677);
#4057=AXIS2_PLACEMENT_3D('',#5985,#4678,#4679);
#4058=AXIS2_PLACEMENT_3D('',#5986,#4680,#4681);
#4059=AXIS2_PLACEMENT_3D('',#5988,#4682,#4683);
#4060=AXIS2_PLACEMENT_3D('',#5992,#4686,#4687);
#4061=AXIS2_PLACEMENT_3D('',#5993,#4688,#4689);
#4062=AXIS2_PLACEMENT_3D('',#5994,#4690,#4691);
#4063=AXIS2_PLACEMENT_3D('',#5996,#4692,#4693);
#4064=AXIS2_PLACEMENT_3D('',#6000,#4696,#4697);
#4065=AXIS2_PLACEMENT_3D('',#6001,#4698,#4699);
#4066=AXIS2_PLACEMENT_3D('',#6002,#4700,#4701);
#4067=AXIS2_PLACEMENT_3D('',#6003,#4702,#4703);
#4068=AXIS2_PLACEMENT_3D('',#6004,#4704,#4705);
#4069=AXIS2_PLACEMENT_3D('',#6006,#4706,#4707);
#4070=AXIS2_PLACEMENT_3D('',#6008,#4708,#4709);
#4071=AXIS2_PLACEMENT_3D('',#6009,#4710,#4711);
#4072=AXIS2_PLACEMENT_3D('',#6012,#4713,#4714);
#4073=AXIS2_PLACEMENT_3D('',#6013,#4715,#4716);
#4074=AXIS2_PLACEMENT_3D('',#6014,#4717,#4718);
#4075=AXIS2_PLACEMENT_3D('',#6016,#4719,#4720);
#4076=AXIS2_PLACEMENT_3D('',#6018,#4722,#4723);
#4077=AXIS2_PLACEMENT_3D('',#6019,#4724,#4725);
#4078=AXIS2_PLACEMENT_3D('',#6020,#4726,#4727);
#4079=AXIS2_PLACEMENT_3D('',#6022,#4728,#4729);
#4080=AXIS2_PLACEMENT_3D('',#6025,#4731,#4732);
#4081=AXIS2_PLACEMENT_3D('',#6026,#4733,#4734);
#4082=AXIS2_PLACEMENT_3D('',#6028,#4735,#4736);
#4083=AXIS2_PLACEMENT_3D('',#6031,#4738,#4739);
#4084=AXIS2_PLACEMENT_3D('',#6032,#4740,#4741);
#4085=AXIS2_PLACEMENT_3D('',#6033,#4742,#4743);
#4086=AXIS2_PLACEMENT_3D('',#6034,#4744,#4745);
#4087=AXIS2_PLACEMENT_3D('',#6035,#4746,#4747);
#4088=AXIS2_PLACEMENT_3D('',#6037,#4748,#4749);
#4089=AXIS2_PLACEMENT_3D('',#6039,#4750,#4751);
#4090=AXIS2_PLACEMENT_3D('',#6040,#4752,#4753);
#4091=AXIS2_PLACEMENT_3D('',#6042,#4754,#4755);
#4092=AXIS2_PLACEMENT_3D('',#6044,#4757,#4758);
#4093=AXIS2_PLACEMENT_3D('',#6046,#4759,#4760);
#4094=AXIS2_PLACEMENT_3D('',#6048,#4761,#4762);
#4095=AXIS2_PLACEMENT_3D('',#6049,#4763,#4764);
#4096=AXIS2_PLACEMENT_3D('',#6051,#4765,#4766);
#4097=AXIS2_PLACEMENT_3D('',#6053,#4767,#4768);
#4098=AXIS2_PLACEMENT_3D('',#6054,#4769,#4770);
#4099=AXIS2_PLACEMENT_3D('',#6056,#4772,#4773);
#4100=AXIS2_PLACEMENT_3D('',#6059,#4775,#4776);
#4101=AXIS2_PLACEMENT_3D('',#6060,#4777,#4778);
#4102=AXIS2_PLACEMENT_3D('',#6062,#4780,#4781);
#4103=AXIS2_PLACEMENT_3D('',#6063,#4782,#4783);
#4104=AXIS2_PLACEMENT_3D('',#6065,#4784,#4785);
#4105=AXIS2_PLACEMENT_3D('',#6068,#4787,#4788);
#4106=AXIS2_PLACEMENT_3D('',#6069,#4789,#4790);
#4107=AXIS2_PLACEMENT_3D('',#6070,#4791,#4792);
#4108=AXIS2_PLACEMENT_3D('',#6071,#4793,#4794);
#4109=AXIS2_PLACEMENT_3D('',#6744,#4795,#4796);
#4110=AXIS2_PLACEMENT_3D('',#6807,#4797,#4798);
#4111=AXIS2_PLACEMENT_3D('',#6808,#4799,#4800);
#4112=AXIS2_PLACEMENT_3D('',#6809,#4801,#4802);
#4113=AXIS2_PLACEMENT_3D('',#6810,#4803,#4804);
#4114=AXIS2_PLACEMENT_3D('',#6811,#4805,#4806);
#4115=AXIS2_PLACEMENT_3D('',#6813,#4807,#4808);
#4116=AXIS2_PLACEMENT_3D('',#6816,#4810,#4811);
#4117=AXIS2_PLACEMENT_3D('',#6817,#4812,#4813);
#4118=AXIS2_PLACEMENT_3D('',#6819,#4814,#4815);
#4119=AXIS2_PLACEMENT_3D('',#6822,#4817,#4818);
#4120=AXIS2_PLACEMENT_3D('',#6823,#4819,#4820);
#4121=AXIS2_PLACEMENT_3D('',#6824,#4821,#4822);
#4122=AXIS2_PLACEMENT_3D('',#6825,#4823,#4824);
#4123=AXIS2_PLACEMENT_3D('',#6826,#4825,#4826);
#4124=AXIS2_PLACEMENT_3D('',#6828,#4827,#4828);
#4125=AXIS2_PLACEMENT_3D('',#6831,#4830,#4831);
#4126=AXIS2_PLACEMENT_3D('',#6832,#4832,#4833);
#4127=AXIS2_PLACEMENT_3D('',#6834,#4834,#4835);
#4128=AXIS2_PLACEMENT_3D('',#6837,#4837,#4838);
#4129=AXIS2_PLACEMENT_3D('',#6838,#4839,#4840);
#4130=AXIS2_PLACEMENT_3D('',#6840,#4841,#4842);
#4131=AXIS2_PLACEMENT_3D('',#6843,#4844,#4845);
#4132=AXIS2_PLACEMENT_3D('',#6844,#4846,#4847);
#4133=AXIS2_PLACEMENT_3D('',#6846,#4848,#4849);
#4134=AXIS2_PLACEMENT_3D('',#6849,#4851,#4852);
#4135=AXIS2_PLACEMENT_3D('',#6850,#4853,#4854);
#4136=AXIS2_PLACEMENT_3D('',#6852,#4855,#4856);
#4137=AXIS2_PLACEMENT_3D('',#6855,#4858,#4859);
#4138=AXIS2_PLACEMENT_3D('',#6856,#4860,#4861);
#4139=AXIS2_PLACEMENT_3D('',#6858,#4862,#4863);
#4140=AXIS2_PLACEMENT_3D('',#6861,#4865,#4866);
#4141=AXIS2_PLACEMENT_3D('',#6862,#4867,#4868);
#4142=AXIS2_PLACEMENT_3D('',#6864,#4869,#4870);
#4143=AXIS2_PLACEMENT_3D('',#6867,#4872,#4873);
#4144=AXIS2_PLACEMENT_3D('',#6868,#4874,#4875);
#4145=AXIS2_PLACEMENT_3D('',#6870,#4876,#4877);
#4146=AXIS2_PLACEMENT_3D('',#6873,#4879,#4880);
#4147=AXIS2_PLACEMENT_3D('',#6874,#4881,#4882);
#4148=AXIS2_PLACEMENT_3D('',#6875,#4883,#4884);
#4149=AXIS2_PLACEMENT_3D('',#6876,#4885,#4886);
#4150=AXIS2_PLACEMENT_3D('',#6877,#4887,#4888);
#4151=AXIS2_PLACEMENT_3D('',#6879,#4889,#4890);
#4152=AXIS2_PLACEMENT_3D('',#6882,#4892,#4893);
#4153=AXIS2_PLACEMENT_3D('',#6883,#4894,#4895);
#4154=AXIS2_PLACEMENT_3D('',#6885,#4896,#4897);
#4155=AXIS2_PLACEMENT_3D('',#6888,#4899,#4900);
#4156=AXIS2_PLACEMENT_3D('',#6889,#4901,#4902);
#4157=AXIS2_PLACEMENT_3D('',#6890,#4903,#4904);
#4158=AXIS2_PLACEMENT_3D('',#6892,#4905,#4906);
#4159=AXIS2_PLACEMENT_3D('',#6893,#4907,#4908);
#4160=AXIS2_PLACEMENT_3D('',#6895,#4909,#4910);
#4161=AXIS2_PLACEMENT_3D('',#6898,#4912,#4913);
#4162=AXIS2_PLACEMENT_3D('',#6899,#4914,#4915);
#4163=AXIS2_PLACEMENT_3D('',#6902,#4917,#4918);
#4164=AXIS2_PLACEMENT_3D('',#6903,#4919,#4920);
#4165=AXIS2_PLACEMENT_3D('',#6904,#4921,#4922);
#4166=AXIS2_PLACEMENT_3D('',#6905,#4923,#4924);
#4167=AXIS2_PLACEMENT_3D('',#6906,#4925,#4926);
#4168=AXIS2_PLACEMENT_3D('',#6909,#4927,#4928);
#4169=AXIS2_PLACEMENT_3D('',#6910,#4929,#4930);
#4170=AXIS2_PLACEMENT_3D('',#6911,#4931,#4932);
#4171=AXIS2_PLACEMENT_3D('',#6915,#4934,#4935);
#4172=AXIS2_PLACEMENT_3D('',#6917,#4937,#4938);
#4173=AXIS2_PLACEMENT_3D('',#6922,#4940,#4941);
#4174=AXIS2_PLACEMENT_3D('',#6925,#4943,#4944);
#4175=AXIS2_PLACEMENT_3D('',#6926,#4945,#4946);
#4176=AXIS2_PLACEMENT_3D('',#6927,#4947,#4948);
#4177=AXIS2_PLACEMENT_3D('',#6928,#4949,#4950);
#4178=AXIS2_PLACEMENT_3D('',#6931,#4951,#4952);
#4179=AXIS2_PLACEMENT_3D('',#6932,#4953,#4954);
#4180=AXIS2_PLACEMENT_3D('',#6933,#4955,#4956);
#4181=AXIS2_PLACEMENT_3D('',#6937,#4958,#4959);
#4182=AXIS2_PLACEMENT_3D('',#6939,#4961,#4962);
#4183=AXIS2_PLACEMENT_3D('',#6942,#4963,#4964);
#4184=AXIS2_PLACEMENT_3D('',#6943,#4965,#4966);
#4185=AXIS2_PLACEMENT_3D('',#6944,#4967,#4968);
#4186=AXIS2_PLACEMENT_3D('',#6948,#4970,#4971);
#4187=AXIS2_PLACEMENT_3D('',#6950,#4973,#4974);
#4188=AXIS2_PLACEMENT_3D('',#6953,#4975,#4976);
#4189=AXIS2_PLACEMENT_3D('',#6954,#4977,#4978);
#4190=AXIS2_PLACEMENT_3D('',#6955,#4979,#4980);
#4191=AXIS2_PLACEMENT_3D('',#6959,#4982,#4983);
#4192=AXIS2_PLACEMENT_3D('',#6961,#4985,#4986);
#4193=AXIS2_PLACEMENT_3D('',#6966,#4988,#4989);
#4194=AXIS2_PLACEMENT_3D('',#6969,#4991,#4992);
#4195=AXIS2_PLACEMENT_3D('',#6970,#4993,#4994);
#4196=AXIS2_PLACEMENT_3D('',#6971,#4995,#4996);
#4197=AXIS2_PLACEMENT_3D('',#6972,#4997,#4998);
#4198=AXIS2_PLACEMENT_3D('',#6974,#4999,#5000);
#4199=AXIS2_PLACEMENT_3D('',#6977,#5002,#5003);
#4200=AXIS2_PLACEMENT_3D('',#6978,#5004,#5005);
#4201=AXIS2_PLACEMENT_3D('',#6979,#5006,#5007);
#4202=AXIS2_PLACEMENT_3D('',#6980,#5008,#5009);
#4203=AXIS2_PLACEMENT_3D('',#6981,#5010,#5011);
#4204=AXIS2_PLACEMENT_3D('',#6982,#5012,#5013);
#4205=AXIS2_PLACEMENT_3D('',#6983,#5014,#5015);
#4206=AXIS2_PLACEMENT_3D('',#6984,#5016,#5017);
#4207=AXIS2_PLACEMENT_3D('',#6986,#5018,#5019);
#4208=AXIS2_PLACEMENT_3D('',#6989,#5021,#5022);
#4209=AXIS2_PLACEMENT_3D('',#6990,#5023,#5024);
#4210=AXIS2_PLACEMENT_3D('',#6992,#5025,#5026);
#4211=AXIS2_PLACEMENT_3D('',#6995,#5028,#5029);
#4212=AXIS2_PLACEMENT_3D('',#6996,#5030,#5031);
#4213=AXIS2_PLACEMENT_3D('',#6998,#5032,#5033);
#4214=AXIS2_PLACEMENT_3D('',#7001,#5035,#5036);
#4215=AXIS2_PLACEMENT_3D('',#7002,#5037,#5038);
#4216=AXIS2_PLACEMENT_3D('',#7004,#5039,#5040);
#4217=AXIS2_PLACEMENT_3D('',#7007,#5042,#5043);
#4218=AXIS2_PLACEMENT_3D('',#7008,#5044,#5045);
#4219=AXIS2_PLACEMENT_3D('',#7010,#5046,#5047);
#4220=AXIS2_PLACEMENT_3D('',#7013,#5049,#5050);
#4221=AXIS2_PLACEMENT_3D('',#7014,#5051,#5052);
#4222=AXIS2_PLACEMENT_3D('',#7016,#5053,#5054);
#4223=AXIS2_PLACEMENT_3D('',#7019,#5056,#5057);
#4224=AXIS2_PLACEMENT_3D('',#7020,#5058,#5059);
#4225=AXIS2_PLACEMENT_3D('',#7022,#5060,#5061);
#4226=AXIS2_PLACEMENT_3D('',#7025,#5063,#5064);
#4227=AXIS2_PLACEMENT_3D('',#7026,#5065,#5066);
#4228=AXIS2_PLACEMENT_3D('',#7028,#5067,#5068);
#4229=AXIS2_PLACEMENT_3D('',#7031,#5070,#5071);
#4230=AXIS2_PLACEMENT_3D('',#7032,#5072,#5073);
#4231=AXIS2_PLACEMENT_3D('',#7033,#5074,#5075);
#4232=AXIS2_PLACEMENT_3D('',#7034,#5076,#5077);
#4233=AXIS2_PLACEMENT_3D('',#7036,#5078,#5079);
#4234=AXIS2_PLACEMENT_3D('',#7039,#5081,#5082);
#4235=AXIS2_PLACEMENT_3D('',#7040,#5083,#5084);
#4236=AXIS2_PLACEMENT_3D('',#7041,#5085,#5086);
#4237=AXIS2_PLACEMENT_3D('',#7042,#5087,#5088);
#4238=AXIS2_PLACEMENT_3D('',#7754,#5089,#5090);
#4239=AXIS2_PLACEMENT_3D('',#7827,#5091,#5092);
#4240=AXIS2_PLACEMENT_3D('',#7828,#5093,#5094);
#4241=AXIS2_PLACEMENT_3D('',#7829,#5095,#5096);
#4242=AXIS2_PLACEMENT_3D('',#7830,#5097,#5098);
#4243=AXIS2_PLACEMENT_3D('',#7831,#5099,#5100);
#4244=AXIS2_PLACEMENT_3D('',#7833,#5101,#5102);
#4245=AXIS2_PLACEMENT_3D('',#7836,#5104,#5105);
#4246=AXIS2_PLACEMENT_3D('',#7837,#5106,#5107);
#4247=AXIS2_PLACEMENT_3D('',#7838,#5108,#5109);
#4248=AXIS2_PLACEMENT_3D('',#7840,#5110,#5111);
#4249=AXIS2_PLACEMENT_3D('',#7843,#5113,#5114);
#4250=AXIS2_PLACEMENT_3D('',#7844,#5115,#5116);
#4251=AXIS2_PLACEMENT_3D('',#7845,#5117,#5118);
#4252=AXIS2_PLACEMENT_3D('',#7846,#5119,#5120);
#4253=AXIS2_PLACEMENT_3D('',#7847,#5121,#5122);
#4254=AXIS2_PLACEMENT_3D('',#7849,#5123,#5124);
#4255=AXIS2_PLACEMENT_3D('',#7852,#5126,#5127);
#4256=AXIS2_PLACEMENT_3D('',#7853,#5128,#5129);
#4257=AXIS2_PLACEMENT_3D('',#7854,#5130,#5131);
#4258=AXIS2_PLACEMENT_3D('',#7855,#5132,#5133);
#4259=AXIS2_PLACEMENT_3D('',#7856,#5134,#5135);
#4260=AXIS2_PLACEMENT_3D('',#7861,#5137,#5138);
#4261=AXIS2_PLACEMENT_3D('',#7862,#5139,#5140);
#4262=AXIS2_PLACEMENT_3D('',#7863,#5141,#5142);
#4263=AXIS2_PLACEMENT_3D('',#7876,#5143,#5144);
#4264=AXIS2_PLACEMENT_3D('',#7923,#5146,#5147);
#4265=AXIS2_PLACEMENT_3D('',#7925,#5149,#5150);
#4266=AXIS2_PLACEMENT_3D('',#7927,#5151,#5152);
#4267=AXIS2_PLACEMENT_3D('',#7930,#5154,#5155);
#4268=AXIS2_PLACEMENT_3D('',#7931,#5156,#5157);
#4269=AXIS2_PLACEMENT_3D('',#7933,#5158,#5159);
#4270=AXIS2_PLACEMENT_3D('',#7936,#5161,#5162);
#4271=AXIS2_PLACEMENT_3D('',#7937,#5163,#5164);
#4272=AXIS2_PLACEMENT_3D('',#7938,#5165,#5166);
#4273=AXIS2_PLACEMENT_3D('',#7939,#5167,#5168);
#4274=AXIS2_PLACEMENT_3D('',#7940,#5169,#5170);
#4275=AXIS2_PLACEMENT_3D('',#7949,#5175,#5176);
#4276=AXIS2_PLACEMENT_3D('',#7955,#5180,#5181);
#4277=AXIS2_PLACEMENT_3D('',#7961,#5185,#5186);
#4278=AXIS2_PLACEMENT_3D('',#7964,#5189,#5190);
#4279=AXIS2_PLACEMENT_3D('',#7965,#5191,#5192);
#4280=AXIS2_PLACEMENT_3D('',#7966,#5193,#5194);
#4281=AXIS2_PLACEMENT_3D('',#7967,#5195,#5196);
#4282=AXIS2_PLACEMENT_3D('',#7976,#5201,#5202);
#4283=AXIS2_PLACEMENT_3D('',#7982,#5206,#5207);
#4284=AXIS2_PLACEMENT_3D('',#7988,#5211,#5212);
#4285=AXIS2_PLACEMENT_3D('',#7991,#5215,#5216);
#4286=AXIS2_PLACEMENT_3D('',#7992,#5217,#5218);
#4287=AXIS2_PLACEMENT_3D('',#7993,#5219,#5220);
#4288=AXIS2_PLACEMENT_3D('',#7994,#5221,#5222);
#4289=AXIS2_PLACEMENT_3D('',#7996,#5223,#5224);
#4290=AXIS2_PLACEMENT_3D('',#7997,#5225,#5226);
#4291=AXIS2_PLACEMENT_3D('',#7999,#5227,#5228);
#4292=AXIS2_PLACEMENT_3D('',#8001,#5230,#5231);
#4293=AXIS2_PLACEMENT_3D('',#8003,#5232,#5233);
#4294=AXIS2_PLACEMENT_3D('',#8005,#5235,#5236);
#4295=AXIS2_PLACEMENT_3D('',#8007,#5237,#5238);
#4296=AXIS2_PLACEMENT_3D('',#8009,#5240,#5241);
#4297=AXIS2_PLACEMENT_3D('',#8011,#5242,#5243);
#4298=AXIS2_PLACEMENT_3D('',#8012,#5244,#5245);
#4299=AXIS2_PLACEMENT_3D('',#8014,#5246,#5247);
#4300=AXIS2_PLACEMENT_3D('',#8016,#5249,#5250);
#4301=AXIS2_PLACEMENT_3D('',#8018,#5251,#5252);
#4302=AXIS2_PLACEMENT_3D('',#8020,#5254,#5255);
#4303=AXIS2_PLACEMENT_3D('',#8022,#5256,#5257);
#4304=AXIS2_PLACEMENT_3D('',#8024,#5259,#5260);
#4305=AXIS2_PLACEMENT_3D('',#8025,#5261,#5262);
#4306=AXIS2_PLACEMENT_3D('',#8034,#5267,#5268);
#4307=AXIS2_PLACEMENT_3D('',#8040,#5272,#5273);
#4308=AXIS2_PLACEMENT_3D('',#8046,#5277,#5278);
#4309=AXIS2_PLACEMENT_3D('',#8052,#5282,#5283);
#4310=AXIS2_PLACEMENT_3D('',#8058,#5287,#5288);
#4311=AXIS2_PLACEMENT_3D('',#8061,#5291,#5292);
#4312=AXIS2_PLACEMENT_3D('',#8062,#5293,#5294);
#4313=AXIS2_PLACEMENT_3D('',#8063,#5295,#5296);
#4314=AXIS2_PLACEMENT_3D('',#8064,#5297,#5298);
#4315=AXIS2_PLACEMENT_3D('',#8078,#5305,#5306);
#4316=AXIS2_PLACEMENT_3D('',#8079,#5307,#5308);
#4317=AXIS2_PLACEMENT_3D('',#8093,#5315,#5316);
#4318=AXIS2_PLACEMENT_3D('',#8094,#5317,#5318);
#4319=AXIS2_PLACEMENT_3D('',#8097,#5321,#5322);
#4320=AXIS2_PLACEMENT_3D('',#8099,#5324,#5325);
#4321=AXIS2_PLACEMENT_3D('',#8101,#5327,#5328);
#4322=AXIS2_PLACEMENT_3D('',#8103,#5330,#5331);
#4323=AXIS2_PLACEMENT_3D('',#8105,#5333,#5334);
#4324=AXIS2_PLACEMENT_3D('',#8106,#5335,#5336);
#4325=AXIS2_PLACEMENT_3D('',#8109,#5338,#5339);
#4326=AXIS2_PLACEMENT_3D('',#8110,#5340,#5341);
#4327=AXIS2_PLACEMENT_3D('',#8112,#5342,#5343);
#4328=AXIS2_PLACEMENT_3D('',#8114,#5344,#5345);
#4329=AXIS2_PLACEMENT_3D('',#8115,#5346,#5347);
#4330=AXIS2_PLACEMENT_3D('',#8117,#5349,#5350);
#4331=AXIS2_PLACEMENT_3D('',#8119,#5351,#5352);
#4332=AXIS2_PLACEMENT_3D('',#8121,#5354,#5355);
#4333=AXIS2_PLACEMENT_3D('',#8123,#5356,#5357);
#4334=AXIS2_PLACEMENT_3D('',#8125,#5359,#5360);
#4335=AXIS2_PLACEMENT_3D('',#8127,#5361,#5362);
#4336=AXIS2_PLACEMENT_3D('',#8128,#5363,#5364);
#4337=AXIS2_PLACEMENT_3D('',#8130,#5366,#5367);
#4338=AXIS2_PLACEMENT_3D('',#8131,#5368,#5369);
#4339=AXIS2_PLACEMENT_3D('',#8133,#5370,#5371);
#4340=AXIS2_PLACEMENT_3D('',#8134,#5372,#5373);
#4341=AXIS2_PLACEMENT_3D('',#8136,#5374,#5375);
#4342=AXIS2_PLACEMENT_3D('',#8138,#5377,#5378);
#4343=AXIS2_PLACEMENT_3D('',#8140,#5379,#5380);
#4344=AXIS2_PLACEMENT_3D('',#8142,#5382,#5383);
#4345=AXIS2_PLACEMENT_3D('',#8144,#5384,#5385);
#4346=AXIS2_PLACEMENT_3D('',#8146,#5387,#5388);
#4347=AXIS2_PLACEMENT_3D('',#8148,#5389,#5390);
#4348=AXIS2_PLACEMENT_3D('',#8149,#5391,#5392);
#4349=AXIS2_PLACEMENT_3D('',#8151,#5393,#5394);
#4350=AXIS2_PLACEMENT_3D('',#8153,#5396,#5397);
#4351=AXIS2_PLACEMENT_3D('',#8155,#5398,#5399);
#4352=AXIS2_PLACEMENT_3D('',#8157,#5401,#5402);
#4353=AXIS2_PLACEMENT_3D('',#8159,#5403,#5404);
#4354=AXIS2_PLACEMENT_3D('',#8161,#5406,#5407);
#4355=AXIS2_PLACEMENT_3D('',#8162,#5408,#5409);
#4356=AXIS2_PLACEMENT_3D('',#8171,#5414,#5415);
#4357=AXIS2_PLACEMENT_3D('',#8177,#5419,#5420);
#4358=AXIS2_PLACEMENT_3D('',#8183,#5424,#5425);
#4359=AXIS2_PLACEMENT_3D('',#8189,#5429,#5430);
#4360=AXIS2_PLACEMENT_3D('',#8195,#5434,#5435);
#4361=AXIS2_PLACEMENT_3D('',#8198,#5438,#5439);
#4362=AXIS2_PLACEMENT_3D('',#8199,#5440,#5441);
#4363=AXIS2_PLACEMENT_3D('',#8200,#5442,#5443);
#4364=AXIS2_PLACEMENT_3D('',#8201,#5444,#5445);
#4365=AXIS2_PLACEMENT_3D('',#8203,#5446,#5447);
#4366=AXIS2_PLACEMENT_3D('',#8206,#5449,#5450);
#4367=AXIS2_PLACEMENT_3D('',#8207,#5451,#5452);
#4368=AXIS2_PLACEMENT_3D('',#8209,#5453,#5454);
#4369=AXIS2_PLACEMENT_3D('',#8212,#5456,#5457);
#4370=AXIS2_PLACEMENT_3D('',#8213,#5458,#5459);
#4371=AXIS2_PLACEMENT_3D('',#8214,#5460,#5461);
#4372=AXIS2_PLACEMENT_3D('',#8215,#5462,#5463);
#4373=AXIS2_PLACEMENT_3D('',#8216,#5464,#5465);
#4374=AXIS2_PLACEMENT_3D('',#8228,#5467,#5468);
#4375=AXIS2_PLACEMENT_3D('',#8244,#5469,#5470);
#4376=AXIS2_PLACEMENT_3D('',#8246,#5471,#5472);
#4377=AXIS2_PLACEMENT_3D('',#8272,#5474,#5475);
#4378=AXIS2_PLACEMENT_3D('',#8275,#5478,#5479);
#4379=AXIS2_PLACEMENT_3D('',#8277,#5481,#5482);
#4380=AXIS2_PLACEMENT_3D('',#8279,#5484,#5485);
#4381=AXIS2_PLACEMENT_3D('',#8281,#5486,#5487);
#4382=AXIS2_PLACEMENT_3D('',#8284,#5489,#5490);
#4383=AXIS2_PLACEMENT_3D('',#8285,#5491,#5492);
#4384=AXIS2_PLACEMENT_3D('',#8287,#5494,#5495);
#4385=AXIS2_PLACEMENT_3D('',#8289,#5497,#5498);
#4386=AXIS2_PLACEMENT_3D('',#8290,#5499,#5500);
#4387=AXIS2_PLACEMENT_3D('',#8291,#5501,#5502);
#4388=AXIS2_PLACEMENT_3D('',#8292,#5503,#5504);
#4389=AXIS2_PLACEMENT_3D('',#8293,#5505,#5506);
#4390=AXIS2_PLACEMENT_3D('',#8302,#5511,#5512);
#4391=AXIS2_PLACEMENT_3D('',#8308,#5516,#5517);
#4392=AXIS2_PLACEMENT_3D('',#8314,#5521,#5522);
#4393=AXIS2_PLACEMENT_3D('',#8320,#5526,#5527);
#4394=AXIS2_PLACEMENT_3D('',#8326,#5531,#5532);
#4395=AXIS2_PLACEMENT_3D('',#8329,#5535,#5536);
#4396=AXIS2_PLACEMENT_3D('',#8330,#5537,#5538);
#4397=AXIS2_PLACEMENT_3D('',#8332,#5539,#5540);
#4398=AXIS2_PLACEMENT_3D('',#8333,#5541,#5542);
#4399=AXIS2_PLACEMENT_3D('',#8335,#5543,#5544);
#4400=AXIS2_PLACEMENT_3D('',#8337,#5546,#5547);
#4401=AXIS2_PLACEMENT_3D('',#8339,#5548,#5549);
#4402=AXIS2_PLACEMENT_3D('',#8341,#5551,#5552);
#4403=AXIS2_PLACEMENT_3D('',#8343,#5553,#5554);
#4404=AXIS2_PLACEMENT_3D('',#8345,#5556,#5557);
#4405=AXIS2_PLACEMENT_3D('',#8346,#5558,#5559);
#4406=AXIS2_PLACEMENT_3D('',#8347,#5560,#5561);
#4407=AXIS2_PLACEMENT_3D('',#8348,#5562,#5563);
#4408=AXIS2_PLACEMENT_3D('',#8349,#5564,#5565);
#4409=AXIS2_PLACEMENT_3D('',#8350,#5566,#5567);
#4410=AXIS2_PLACEMENT_3D('',#8351,#5568,#5569);
#4411=AXIS2_PLACEMENT_3D('',#8352,#5570,#5571);
#4412=AXIS2_PLACEMENT_3D('',#8353,#5572,#5573);
#4413=AXIS2_PLACEMENT_3D('',#8354,#5574,#5575);
#4414=AXIS2_PLACEMENT_3D('',#8355,#5576,#5577);
#4415=AXIS2_PLACEMENT_3D('',#8356,#5578,#5579);
#4416=AXIS2_PLACEMENT_3D('',#8357,#5580,#5581);
#4417=AXIS2_PLACEMENT_3D('',#8358,#5582,#5583);
#4418=AXIS2_PLACEMENT_3D('',#8359,#5584,#5585);
#4419=AXIS2_PLACEMENT_3D('',#8360,#5586,#5587);
#4420=AXIS2_PLACEMENT_3D('',#8361,#5588,#5589);
#4421=AXIS2_PLACEMENT_3D('',#8362,#5590,#5591);
#4422=AXIS2_PLACEMENT_3D('',#8363,#5592,#5593);
#4423=AXIS2_PLACEMENT_3D('',#8364,#5594,#5595);
#4424=AXIS2_PLACEMENT_3D('',#8365,#5596,#5597);
#4425=AXIS2_PLACEMENT_3D('',#8366,#5598,#5599);
#4426=AXIS2_PLACEMENT_3D('',#8367,#5600,#5601);
#4427=AXIS2_PLACEMENT_3D('',#8368,#5602,#5603);
#4428=AXIS2_PLACEMENT_3D('',#8369,#5604,#5605);
#4429=AXIS2_PLACEMENT_3D('',#8370,#5606,#5607);
#4430=AXIS2_PLACEMENT_3D('',#8371,#5608,#5609);
#4431=AXIS2_PLACEMENT_3D('',#8372,#5610,#5611);
#4432=AXIS2_PLACEMENT_3D('',#8373,#5612,#5613);
#4433=AXIS2_PLACEMENT_3D('',#8374,#5614,#5615);
#4434=AXIS2_PLACEMENT_3D('',#8375,#5616,#5617);
#4435=AXIS2_PLACEMENT_3D('',#8376,#5618,#5619);
#4436=DIRECTION('axis',(0.,0.,1.));
#4437=DIRECTION('refdir',(1.,0.,0.));
#4438=DIRECTION('axis',(0.,0.,1.));
#4439=DIRECTION('refdir',(1.,0.,0.));
#4440=DIRECTION('center_axis',(0.,0.,1.));
#4441=DIRECTION('ref_axis',(1.,0.,0.));
#4442=DIRECTION('center_axis',(0.,0.,1.));
#4443=DIRECTION('ref_axis',(1.,0.,0.));
#4444=DIRECTION('',(0.,0.,1.));
#4445=DIRECTION('center_axis',(0.,0.,-1.));
#4446=DIRECTION('ref_axis',(1.,0.,0.));
#4447=DIRECTION('center_axis',(0.,0.,1.));
#4448=DIRECTION('ref_axis',(1.,0.,0.));
#4449=DIRECTION('center_axis',(0.,0.,1.));
#4450=DIRECTION('ref_axis',(1.,0.,0.));
#4451=DIRECTION('',(0.,0.,1.));
#4452=DIRECTION('center_axis',(0.,0.,-1.));
#4453=DIRECTION('ref_axis',(1.,0.,0.));
#4454=DIRECTION('center_axis',(0.,1.,0.));
#4455=DIRECTION('ref_axis',(-1.,0.,0.));
#4456=DIRECTION('',(-1.,0.,0.));
#4457=DIRECTION('',(0.,0.,1.));
#4458=DIRECTION('',(-1.,0.,0.));
#4459=DIRECTION('',(0.,0.,1.));
#4460=DIRECTION('center_axis',(1.,0.,0.));
#4461=DIRECTION('ref_axis',(0.,1.,0.));
#4462=DIRECTION('',(0.,1.,0.));
#4463=DIRECTION('',(0.,1.,0.));
#4464=DIRECTION('',(0.,0.,1.));
#4465=DIRECTION('center_axis',(0.,-1.,0.));
#4466=DIRECTION('ref_axis',(1.,0.,0.));
#4467=DIRECTION('',(1.,0.,0.));
#4468=DIRECTION('',(1.,0.,0.));
#4469=DIRECTION('',(0.,0.,1.));
#4470=DIRECTION('center_axis',(-1.,0.,0.));
#4471=DIRECTION('ref_axis',(0.,-1.,0.));
#4472=DIRECTION('',(0.,-1.,0.));
#4473=DIRECTION('',(0.,-1.,0.));
#4474=DIRECTION('center_axis',(0.,0.,1.));
#4475=DIRECTION('ref_axis',(1.,0.,0.));
#4476=DIRECTION('center_axis',(0.,0.,1.));
#4477=DIRECTION('ref_axis',(1.,0.,0.));
#4478=DIRECTION('axis',(0.,0.,1.));
#4479=DIRECTION('refdir',(1.,0.,0.));
#4480=DIRECTION('center_axis',(0.,0.,1.));
#4481=DIRECTION('ref_axis',(1.,0.,0.));
#4482=DIRECTION('center_axis',(0.,0.,1.));
#4483=DIRECTION('ref_axis',(1.,0.,0.));
#4484=DIRECTION('',(0.,0.,1.));
#4485=DIRECTION('center_axis',(0.,0.,-1.));
#4486=DIRECTION('ref_axis',(1.,0.,0.));
#4487=DIRECTION('center_axis',(0.,1.,0.));
#4488=DIRECTION('ref_axis',(-1.,0.,0.));
#4489=DIRECTION('',(-1.,0.,0.));
#4490=DIRECTION('',(0.,0.,1.));
#4491=DIRECTION('',(-1.,0.,0.));
#4492=DIRECTION('',(0.,0.,1.));
#4493=DIRECTION('center_axis',(1.,0.,0.));
#4494=DIRECTION('ref_axis',(0.,1.,0.));
#4495=DIRECTION('',(0.,1.,0.));
#4496=DIRECTION('',(0.,1.,0.));
#4497=DIRECTION('',(0.,0.,1.));
#4498=DIRECTION('center_axis',(0.,-1.,0.));
#4499=DIRECTION('ref_axis',(1.,0.,0.));
#4500=DIRECTION('',(1.,0.,0.));
#4501=DIRECTION('',(1.,0.,0.));
#4502=DIRECTION('',(0.,0.,1.));
#4503=DIRECTION('center_axis',(-1.,0.,0.));
#4504=DIRECTION('ref_axis',(0.,-1.,0.));
#4505=DIRECTION('',(0.,-1.,0.));
#4506=DIRECTION('',(0.,-1.,0.));
#4507=DIRECTION('center_axis',(0.,0.,1.));
#4508=DIRECTION('ref_axis',(1.,0.,0.));
#4509=DIRECTION('center_axis',(0.,0.,1.));
#4510=DIRECTION('ref_axis',(1.,0.,0.));
#4511=DIRECTION('axis',(0.,0.,1.));
#4512=DIRECTION('refdir',(1.,0.,0.));
#4513=DIRECTION('center_axis',(0.,0.,1.));
#4514=DIRECTION('ref_axis',(1.,0.,0.));
#4515=DIRECTION('center_axis',(0.,0.,1.));
#4516=DIRECTION('ref_axis',(1.,0.,0.));
#4517=DIRECTION('',(0.,0.,1.));
#4518=DIRECTION('center_axis',(0.,0.,-1.));
#4519=DIRECTION('ref_axis',(1.,0.,0.));
#4520=DIRECTION('center_axis',(0.,1.,0.));
#4521=DIRECTION('ref_axis',(-1.,0.,0.));
#4522=DIRECTION('',(-1.,0.,0.));
#4523=DIRECTION('',(0.,0.,1.));
#4524=DIRECTION('',(-1.,0.,0.));
#4525=DIRECTION('',(0.,0.,1.));
#4526=DIRECTION('center_axis',(1.,0.,0.));
#4527=DIRECTION('ref_axis',(0.,1.,0.));
#4528=DIRECTION('',(0.,1.,0.));
#4529=DIRECTION('',(0.,1.,0.));
#4530=DIRECTION('',(0.,0.,1.));
#4531=DIRECTION('center_axis',(0.,-1.,0.));
#4532=DIRECTION('ref_axis',(1.,0.,0.));
#4533=DIRECTION('',(1.,0.,0.));
#4534=DIRECTION('',(1.,0.,0.));
#4535=DIRECTION('',(0.,0.,1.));
#4536=DIRECTION('center_axis',(-1.,0.,0.));
#4537=DIRECTION('ref_axis',(0.,-1.,0.));
#4538=DIRECTION('',(0.,-1.,0.));
#4539=DIRECTION('',(0.,-1.,0.));
#4540=DIRECTION('center_axis',(0.,0.,1.));
#4541=DIRECTION('ref_axis',(1.,0.,0.));
#4542=DIRECTION('center_axis',(0.,0.,1.));
#4543=DIRECTION('ref_axis',(1.,0.,0.));
#4544=DIRECTION('axis',(0.,0.,1.));
#4545=DIRECTION('refdir',(1.,0.,0.));
#4546=DIRECTION('center_axis',(0.,0.,1.));
#4547=DIRECTION('ref_axis',(1.,0.,0.));
#4548=DIRECTION('center_axis',(0.,0.,1.));
#4549=DIRECTION('ref_axis',(1.,0.,0.));
#4550=DIRECTION('',(0.,0.,1.));
#4551=DIRECTION('center_axis',(0.,0.,-1.));
#4552=DIRECTION('ref_axis',(1.,0.,0.));
#4553=DIRECTION('center_axis',(0.,0.,1.));
#4554=DIRECTION('ref_axis',(1.,0.,0.));
#4555=DIRECTION('center_axis',(0.,0.,1.));
#4556=DIRECTION('ref_axis',(1.,0.,0.));
#4557=DIRECTION('center_axis',(0.,0.,1.));
#4558=DIRECTION('ref_axis',(1.,0.,0.));
#4559=DIRECTION('',(0.,0.,1.));
#4560=DIRECTION('center_axis',(0.,0.,-1.));
#4561=DIRECTION('ref_axis',(1.,0.,0.));
#4562=DIRECTION('center_axis',(0.,0.,1.));
#4563=DIRECTION('ref_axis',(1.,0.,0.));
#4564=DIRECTION('center_axis',(0.,0.,1.));
#4565=DIRECTION('ref_axis',(1.,0.,0.));
#4566=DIRECTION('center_axis',(0.,0.,1.));
#4567=DIRECTION('ref_axis',(1.,0.,0.));
#4568=DIRECTION('',(0.,0.,1.));
#4569=DIRECTION('center_axis',(0.,0.,-1.));
#4570=DIRECTION('ref_axis',(1.,0.,0.));
#4571=DIRECTION('center_axis',(0.,0.,1.));
#4572=DIRECTION('ref_axis',(1.,0.,0.));
#4573=DIRECTION('center_axis',(0.,0.,1.));
#4574=DIRECTION('ref_axis',(1.,0.,0.));
#4575=DIRECTION('center_axis',(0.,0.,1.));
#4576=DIRECTION('ref_axis',(1.,0.,0.));
#4577=DIRECTION('',(0.,0.,1.));
#4578=DIRECTION('center_axis',(0.,0.,-1.));
#4579=DIRECTION('ref_axis',(1.,0.,0.));
#4580=DIRECTION('center_axis',(0.,0.,1.));
#4581=DIRECTION('ref_axis',(1.,0.,0.));
#4582=DIRECTION('center_axis',(0.,0.,1.));
#4583=DIRECTION('ref_axis',(1.,0.,0.));
#4584=DIRECTION('center_axis',(0.,0.,1.));
#4585=DIRECTION('ref_axis',(1.,0.,0.));
#4586=DIRECTION('',(0.,0.,1.));
#4587=DIRECTION('center_axis',(0.,0.,-1.));
#4588=DIRECTION('ref_axis',(1.,0.,0.));
#4589=DIRECTION('center_axis',(0.,0.,1.));
#4590=DIRECTION('ref_axis',(1.,0.,0.));
#4591=DIRECTION('center_axis',(0.,0.,1.));
#4592=DIRECTION('ref_axis',(1.,0.,0.));
#4593=DIRECTION('center_axis',(0.,0.,1.));
#4594=DIRECTION('ref_axis',(1.,0.,0.));
#4595=DIRECTION('',(0.,0.,1.));
#4596=DIRECTION('center_axis',(0.,0.,-1.));
#4597=DIRECTION('ref_axis',(1.,0.,0.));
#4598=DIRECTION('center_axis',(0.,0.,1.));
#4599=DIRECTION('ref_axis',(1.,0.,0.));
#4600=DIRECTION('center_axis',(1.,0.,0.));
#4601=DIRECTION('ref_axis',(0.,0.,-1.));
#4602=DIRECTION('center_axis',(-1.,0.,0.));
#4603=DIRECTION('ref_axis',(0.,0.,-1.));
#4604=DIRECTION('center_axis',(1.,0.,0.));
#4605=DIRECTION('ref_axis',(0.,0.,-1.));
#4606=DIRECTION('center_axis',(-1.,0.,0.));
#4607=DIRECTION('ref_axis',(0.,0.,-1.));
#4608=DIRECTION('center_axis',(1.,0.,0.));
#4609=DIRECTION('ref_axis',(0.,0.,-1.));
#4610=DIRECTION('',(0.,0.,-1.));
#4611=DIRECTION('center_axis',(1.,0.,0.));
#4612=DIRECTION('ref_axis',(0.,0.,-1.));
#4613=DIRECTION('',(0.,0.,-1.));
#4614=DIRECTION('center_axis',(1.,0.,0.));
#4615=DIRECTION('ref_axis',(0.,0.,-1.));
#4616=DIRECTION('',(0.,0.,-1.));
#4617=DIRECTION('center_axis',(1.,0.,0.));
#4618=DIRECTION('ref_axis',(0.,0.,-1.));
#4619=DIRECTION('',(0.,0.,-1.));
#4620=DIRECTION('center_axis',(1.,0.,0.));
#4621=DIRECTION('ref_axis',(0.,0.,-1.));
#4622=DIRECTION('',(1.,0.,0.));
#4623=DIRECTION('center_axis',(1.,0.,0.));
#4624=DIRECTION('ref_axis',(0.,0.,-1.));
#4625=DIRECTION('center_axis',(1.,0.,0.));
#4626=DIRECTION('ref_axis',(0.,0.,-1.));
#4627=DIRECTION('',(1.,0.,0.));
#4628=DIRECTION('',(1.,0.,0.));
#4629=DIRECTION('',(1.,0.,0.));
#4630=DIRECTION('center_axis',(0.,0.,1.));
#4631=DIRECTION('ref_axis',(1.,0.,0.));
#4632=DIRECTION('center_axis',(0.,0.,-1.));
#4633=DIRECTION('ref_axis',(1.,0.,0.));
#4634=DIRECTION('',(0.,0.,1.));
#4635=DIRECTION('center_axis',(0.,0.,1.));
#4636=DIRECTION('ref_axis',(1.,0.,0.));
#4637=DIRECTION('center_axis',(1.,0.,0.));
#4638=DIRECTION('ref_axis',(0.,0.,-1.));
#4639=DIRECTION('',(1.,0.,0.));
#4640=DIRECTION('center_axis',(1.,0.,0.));
#4641=DIRECTION('ref_axis',(0.,0.,-1.));
#4642=DIRECTION('center_axis',(1.,0.,0.));
#4643=DIRECTION('ref_axis',(0.,0.,-1.));
#4644=DIRECTION('center_axis',(0.,0.,1.));
#4645=DIRECTION('ref_axis',(1.,0.,0.));
#4646=DIRECTION('center_axis',(0.,0.,1.));
#4647=DIRECTION('ref_axis',(1.,0.,0.));
#4648=DIRECTION('',(0.,0.,1.));
#4649=DIRECTION('center_axis',(0.,0.,1.));
#4650=DIRECTION('ref_axis',(1.,0.,0.));
#4651=DIRECTION('center_axis',(0.,0.,1.));
#4652=DIRECTION('ref_axis',(1.,0.,0.));
#4653=DIRECTION('center_axis',(0.,0.,1.));
#4654=DIRECTION('ref_axis',(1.,0.,0.));
#4655=DIRECTION('center_axis',(0.,0.,1.));
#4656=DIRECTION('ref_axis',(1.,0.,0.));
#4657=DIRECTION('',(0.,0.,1.));
#4658=DIRECTION('center_axis',(0.,0.,1.));
#4659=DIRECTION('ref_axis',(1.,0.,0.));
#4660=DIRECTION('center_axis',(0.,0.,1.));
#4661=DIRECTION('ref_axis',(1.,0.,0.));
#4662=DIRECTION('center_axis',(0.,0.,1.));
#4663=DIRECTION('ref_axis',(1.,0.,0.));
#4664=DIRECTION('center_axis',(0.,0.,1.));
#4665=DIRECTION('ref_axis',(1.,0.,0.));
#4666=DIRECTION('',(0.,0.,1.));
#4667=DIRECTION('center_axis',(0.,0.,1.));
#4668=DIRECTION('ref_axis',(1.,0.,0.));
#4669=DIRECTION('center_axis',(0.,0.,1.));
#4670=DIRECTION('ref_axis',(1.,0.,0.));
#4671=DIRECTION('center_axis',(0.,0.,1.));
#4672=DIRECTION('ref_axis',(1.,0.,0.));
#4673=DIRECTION('center_axis',(0.,0.,1.));
#4674=DIRECTION('ref_axis',(1.,0.,0.));
#4675=DIRECTION('',(0.,0.,1.));
#4676=DIRECTION('center_axis',(0.,0.,-1.));
#4677=DIRECTION('ref_axis',(1.,0.,0.));
#4678=DIRECTION('center_axis',(0.,0.,1.));
#4679=DIRECTION('ref_axis',(1.,0.,0.));
#4680=DIRECTION('center_axis',(0.,0.,1.));
#4681=DIRECTION('ref_axis',(-1.,1.22464679914735E-16,0.));
#4682=DIRECTION('center_axis',(0.,0.,1.));
#4683=DIRECTION('ref_axis',(1.,0.,0.));
#4684=DIRECTION('',(0.,0.,1.));
#4685=DIRECTION('',(0.,0.,1.));
#4686=DIRECTION('center_axis',(0.,0.,-1.));
#4687=DIRECTION('ref_axis',(1.,0.,0.));
#4688=DIRECTION('center_axis',(0.,0.,1.));
#4689=DIRECTION('ref_axis',(1.,0.,0.));
#4690=DIRECTION('center_axis',(0.,0.,1.));
#4691=DIRECTION('ref_axis',(1.,0.,0.));
#4692=DIRECTION('center_axis',(0.,0.,1.));
#4693=DIRECTION('ref_axis',(1.,0.,0.));
#4694=DIRECTION('',(0.,0.,-1.));
#4695=DIRECTION('',(0.,0.,-1.));
#4696=DIRECTION('center_axis',(0.,0.,1.));
#4697=DIRECTION('ref_axis',(1.,0.,0.));
#4698=DIRECTION('center_axis',(0.,0.,1.));
#4699=DIRECTION('ref_axis',(1.,0.,0.));
#4700=DIRECTION('center_axis',(0.,0.,1.));
#4701=DIRECTION('ref_axis',(1.,0.,0.));
#4702=DIRECTION('axis',(0.,0.,1.));
#4703=DIRECTION('refdir',(1.,0.,0.));
#4704=DIRECTION('center_axis',(0.,0.,1.));
#4705=DIRECTION('ref_axis',(1.,0.,0.));
#4706=DIRECTION('center_axis',(0.,0.,1.));
#4707=DIRECTION('ref_axis',(1.,0.,0.));
#4708=DIRECTION('center_axis',(0.,0.,1.));
#4709=DIRECTION('ref_axis',(1.,0.,0.));
#4710=DIRECTION('center_axis',(0.,0.,1.));
#4711=DIRECTION('ref_axis',(1.,0.,0.));
#4712=DIRECTION('',(0.,0.,-1.));
#4713=DIRECTION('center_axis',(0.,0.,1.));
#4714=DIRECTION('ref_axis',(1.,0.,0.));
#4715=DIRECTION('center_axis',(0.,0.,1.));
#4716=DIRECTION('ref_axis',(1.,0.,0.));
#4717=DIRECTION('center_axis',(0.,0.,1.));
#4718=DIRECTION('ref_axis',(1.,0.,0.));
#4719=DIRECTION('center_axis',(0.,0.,1.));
#4720=DIRECTION('ref_axis',(1.,0.,0.));
#4721=DIRECTION('',(0.,0.,-1.));
#4722=DIRECTION('center_axis',(0.,0.,1.));
#4723=DIRECTION('ref_axis',(1.,0.,0.));
#4724=DIRECTION('axis',(0.,0.,1.));
#4725=DIRECTION('refdir',(1.,0.,0.));
#4726=DIRECTION('center_axis',(0.,0.,1.));
#4727=DIRECTION('ref_axis',(1.,0.,0.));
#4728=DIRECTION('center_axis',(0.,0.,-1.));
#4729=DIRECTION('ref_axis',(1.,0.,0.));
#4730=DIRECTION('',(0.,0.,-1.));
#4731=DIRECTION('center_axis',(0.,0.,-1.));
#4732=DIRECTION('ref_axis',(1.,0.,0.));
#4733=DIRECTION('center_axis',(0.,0.,1.));
#4734=DIRECTION('ref_axis',(1.,0.,0.));
#4735=DIRECTION('center_axis',(0.,0.,1.));
#4736=DIRECTION('ref_axis',(1.,0.,0.));
#4737=DIRECTION('',(0.,0.,-1.));
#4738=DIRECTION('center_axis',(0.,0.,1.));
#4739=DIRECTION('ref_axis',(1.,0.,0.));
#4740=DIRECTION('center_axis',(0.,0.,1.));
#4741=DIRECTION('ref_axis',(1.,0.,0.));
#4742=DIRECTION('center_axis',(0.,0.,1.));
#4743=DIRECTION('ref_axis',(1.,0.,0.));
#4744=DIRECTION('axis',(0.,0.,1.));
#4745=DIRECTION('refdir',(1.,0.,0.));
#4746=DIRECTION('center_axis',(0.,0.,1.));
#4747=DIRECTION('ref_axis',(1.,0.,0.));
#4748=DIRECTION('center_axis',(0.,0.,1.));
#4749=DIRECTION('ref_axis',(1.,0.,0.));
#4750=DIRECTION('center_axis',(0.,0.,-1.));
#4751=DIRECTION('ref_axis',(1.,0.,0.));
#4752=DIRECTION('center_axis',(0.,0.,1.));
#4753=DIRECTION('ref_axis',(1.,0.,0.));
#4754=DIRECTION('center_axis',(0.,0.,1.));
#4755=DIRECTION('ref_axis',(1.,0.,0.));
#4756=DIRECTION('',(0.,0.,-1.));
#4757=DIRECTION('center_axis',(0.,0.,1.));
#4758=DIRECTION('ref_axis',(1.,0.,0.));
#4759=DIRECTION('center_axis',(0.,0.,1.));
#4760=DIRECTION('ref_axis',(1.,0.,0.));
#4761=DIRECTION('center_axis',(0.,0.,1.));
#4762=DIRECTION('ref_axis',(1.,0.,0.));
#4763=DIRECTION('center_axis',(0.,0.,1.));
#4764=DIRECTION('ref_axis',(1.,0.,0.));
#4765=DIRECTION('center_axis',(0.,0.,1.));
#4766=DIRECTION('ref_axis',(1.,0.,0.));
#4767=DIRECTION('center_axis',(0.,0.,-1.));
#4768=DIRECTION('ref_axis',(1.,0.,0.));
#4769=DIRECTION('center_axis',(0.,0.,1.));
#4770=DIRECTION('ref_axis',(1.,0.,0.));
#4771=DIRECTION('',(0.,0.,-1.));
#4772=DIRECTION('center_axis',(0.,0.,1.));
#4773=DIRECTION('ref_axis',(1.,0.,0.));
#4774=DIRECTION('',(0.,0.,-1.));
#4775=DIRECTION('center_axis',(0.,0.,-1.));
#4776=DIRECTION('ref_axis',(1.,0.,0.));
#4777=DIRECTION('center_axis',(0.,0.,1.));
#4778=DIRECTION('ref_axis',(1.,0.,0.));
#4779=DIRECTION('',(0.,0.,-1.));
#4780=DIRECTION('center_axis',(0.,0.,1.));
#4781=DIRECTION('ref_axis',(1.,0.,0.));
#4782=DIRECTION('center_axis',(0.,0.,1.));
#4783=DIRECTION('ref_axis',(1.,0.,0.));
#4784=DIRECTION('center_axis',(0.,0.,1.));
#4785=DIRECTION('ref_axis',(1.,0.,0.));
#4786=DIRECTION('',(0.,0.,-1.));
#4787=DIRECTION('center_axis',(0.,0.,1.));
#4788=DIRECTION('ref_axis',(1.,0.,0.));
#4789=DIRECTION('center_axis',(0.,0.,1.));
#4790=DIRECTION('ref_axis',(1.,0.,0.));
#4791=DIRECTION('center_axis',(0.,0.,1.));
#4792=DIRECTION('ref_axis',(1.,0.,0.));
#4793=DIRECTION('axis',(0.,0.,1.));
#4794=DIRECTION('refdir',(1.,0.,0.));
#4795=DIRECTION('center_axis',(-0.000134706207972677,0.996949949346912,
0.0780434516883255));
#4796=DIRECTION('ref_axis',(1.0545100428422E-5,-0.0780434509759074,0.99694995844755));
#4797=DIRECTION('center_axis',(0.000134706099743608,0.996949949299701,0.0780434522915993));
#4798=DIRECTION('ref_axis',(-0.630738728235735,0.0606460551105772,-0.77362181503826));
#4799=DIRECTION('center_axis',(0.000134706099743608,0.996949949299701,0.0780434522915993));
#4800=DIRECTION('ref_axis',(-0.630738728235735,0.0606460551105772,-0.77362181503826));
#4801=DIRECTION('center_axis',(-0.000134706207972677,0.996949949346912,
0.0780434516883255));
#4802=DIRECTION('ref_axis',(1.0545100428422E-5,-0.0780434509759074,0.99694995844755));
#4803=DIRECTION('axis',(0.,0.,1.));
#4804=DIRECTION('refdir',(1.,0.,0.));
#4805=DIRECTION('center_axis',(0.,0.,1.));
#4806=DIRECTION('ref_axis',(1.,0.,0.));
#4807=DIRECTION('center_axis',(0.,0.,-1.));
#4808=DIRECTION('ref_axis',(1.,0.,0.));
#4809=DIRECTION('',(0.,0.,-1.));
#4810=DIRECTION('center_axis',(0.,0.,-1.));
#4811=DIRECTION('ref_axis',(1.,0.,0.));
#4812=DIRECTION('center_axis',(0.,0.,1.));
#4813=DIRECTION('ref_axis',(1.,0.,0.));
#4814=DIRECTION('center_axis',(0.,0.,1.));
#4815=DIRECTION('ref_axis',(1.,0.,0.));
#4816=DIRECTION('',(0.,0.,-1.));
#4817=DIRECTION('center_axis',(0.,0.,1.));
#4818=DIRECTION('ref_axis',(1.,0.,0.));
#4819=DIRECTION('center_axis',(0.,0.,1.));
#4820=DIRECTION('ref_axis',(1.,0.,0.));
#4821=DIRECTION('center_axis',(0.,0.,1.));
#4822=DIRECTION('ref_axis',(1.,0.,0.));
#4823=DIRECTION('axis',(0.,0.,1.));
#4824=DIRECTION('refdir',(1.,0.,0.));
#4825=DIRECTION('center_axis',(0.,0.,1.));
#4826=DIRECTION('ref_axis',(1.,0.,0.));
#4827=DIRECTION('center_axis',(0.,0.,1.));
#4828=DIRECTION('ref_axis',(1.,0.,0.));
#4829=DIRECTION('',(0.,0.,1.));
#4830=DIRECTION('center_axis',(0.,0.,-1.));
#4831=DIRECTION('ref_axis',(1.,0.,0.));
#4832=DIRECTION('center_axis',(0.,0.,1.));
#4833=DIRECTION('ref_axis',(1.,0.,0.));
#4834=DIRECTION('center_axis',(0.,0.,1.));
#4835=DIRECTION('ref_axis',(1.,0.,0.));
#4836=DIRECTION('',(0.,0.,1.));
#4837=DIRECTION('center_axis',(0.,0.,-1.));
#4838=DIRECTION('ref_axis',(1.,0.,0.));
#4839=DIRECTION('center_axis',(0.,0.,1.));
#4840=DIRECTION('ref_axis',(1.,0.,0.));
#4841=DIRECTION('center_axis',(0.,0.,1.));
#4842=DIRECTION('ref_axis',(1.,0.,0.));
#4843=DIRECTION('',(0.,0.,1.));
#4844=DIRECTION('center_axis',(0.,0.,-1.));
#4845=DIRECTION('ref_axis',(1.,0.,0.));
#4846=DIRECTION('center_axis',(0.,0.,1.));
#4847=DIRECTION('ref_axis',(1.,0.,0.));
#4848=DIRECTION('center_axis',(0.,0.,1.));
#4849=DIRECTION('ref_axis',(1.,0.,0.));
#4850=DIRECTION('',(0.,0.,1.));
#4851=DIRECTION('center_axis',(0.,0.,-1.));
#4852=DIRECTION('ref_axis',(1.,0.,0.));
#4853=DIRECTION('center_axis',(0.,0.,1.));
#4854=DIRECTION('ref_axis',(1.,0.,0.));
#4855=DIRECTION('center_axis',(0.,0.,1.));
#4856=DIRECTION('ref_axis',(1.,0.,0.));
#4857=DIRECTION('',(0.,0.,1.));
#4858=DIRECTION('center_axis',(0.,0.,-1.));
#4859=DIRECTION('ref_axis',(1.,0.,0.));
#4860=DIRECTION('center_axis',(0.,0.,1.));
#4861=DIRECTION('ref_axis',(1.,0.,0.));
#4862=DIRECTION('center_axis',(0.,0.,1.));
#4863=DIRECTION('ref_axis',(1.,0.,0.));
#4864=DIRECTION('',(0.,0.,1.));
#4865=DIRECTION('center_axis',(0.,0.,-1.));
#4866=DIRECTION('ref_axis',(1.,0.,0.));
#4867=DIRECTION('center_axis',(0.,0.,1.));
#4868=DIRECTION('ref_axis',(1.,0.,0.));
#4869=DIRECTION('center_axis',(0.,0.,-1.));
#4870=DIRECTION('ref_axis',(1.,0.,0.));
#4871=DIRECTION('',(0.,0.,-1.));
#4872=DIRECTION('center_axis',(0.,0.,-1.));
#4873=DIRECTION('ref_axis',(1.,0.,0.));
#4874=DIRECTION('center_axis',(0.,0.,1.));
#4875=DIRECTION('ref_axis',(1.,0.,0.));
#4876=DIRECTION('center_axis',(0.,0.,1.));
#4877=DIRECTION('ref_axis',(1.,0.,0.));
#4878=DIRECTION('',(0.,0.,-1.));
#4879=DIRECTION('center_axis',(0.,0.,1.));
#4880=DIRECTION('ref_axis',(1.,0.,0.));
#4881=DIRECTION('center_axis',(0.,0.,1.));
#4882=DIRECTION('ref_axis',(1.,0.,0.));
#4883=DIRECTION('center_axis',(0.,0.,1.));
#4884=DIRECTION('ref_axis',(1.,0.,0.));
#4885=DIRECTION('axis',(0.,0.,1.));
#4886=DIRECTION('refdir',(1.,0.,0.));
#4887=DIRECTION('center_axis',(0.,0.,1.));
#4888=DIRECTION('ref_axis',(1.,0.,0.));
#4889=DIRECTION('center_axis',(0.,0.,-1.));
#4890=DIRECTION('ref_axis',(1.,0.,0.));
#4891=DIRECTION('',(0.,0.,-1.));
#4892=DIRECTION('center_axis',(0.,0.,1.));
#4893=DIRECTION('ref_axis',(1.,0.,0.));
#4894=DIRECTION('center_axis',(0.,0.,1.));
#4895=DIRECTION('ref_axis',(1.,0.,0.));
#4896=DIRECTION('center_axis',(0.,0.,1.));
#4897=DIRECTION('ref_axis',(1.,0.,0.));
#4898=DIRECTION('',(0.,0.,-1.));
#4899=DIRECTION('center_axis',(0.,0.,-1.));
#4900=DIRECTION('ref_axis',(1.,0.,0.));
#4901=DIRECTION('center_axis',(0.,0.,1.));
#4902=DIRECTION('ref_axis',(1.,0.,0.));
#4903=DIRECTION('center_axis',(0.,0.,1.));
#4904=DIRECTION('ref_axis',(1.,0.,0.));
#4905=DIRECTION('center_axis',(0.,0.,1.));
#4906=DIRECTION('ref_axis',(1.,0.,0.));
#4907=DIRECTION('center_axis',(0.,0.,1.));
#4908=DIRECTION('ref_axis',(1.,0.,0.));
#4909=DIRECTION('center_axis',(0.,0.,-1.));
#4910=DIRECTION('ref_axis',(1.,0.,0.));
#4911=DIRECTION('',(0.,0.,-1.));
#4912=DIRECTION('center_axis',(0.,0.,-1.));
#4913=DIRECTION('ref_axis',(1.,0.,0.));
#4914=DIRECTION('center_axis',(0.,0.,1.));
#4915=DIRECTION('ref_axis',(1.,0.,0.));
#4916=DIRECTION('',(0.,0.,-1.));
#4917=DIRECTION('center_axis',(0.,0.,1.));
#4918=DIRECTION('ref_axis',(1.,0.,0.));
#4919=DIRECTION('center_axis',(0.,0.,1.));
#4920=DIRECTION('ref_axis',(1.,0.,0.));
#4921=DIRECTION('center_axis',(0.,0.,1.));
#4922=DIRECTION('ref_axis',(1.,0.,0.));
#4923=DIRECTION('axis',(0.,0.,1.));
#4924=DIRECTION('refdir',(1.,0.,0.));
#4925=DIRECTION('center_axis',(0.,0.,1.));
#4926=DIRECTION('ref_axis',(1.,0.,0.));
#4927=DIRECTION('center_axis',(0.,0.,1.));
#4928=DIRECTION('ref_axis',(1.,0.,0.));
#4929=DIRECTION('center_axis',(0.,0.,1.));
#4930=DIRECTION('ref_axis',(1.,0.,0.));
#4931=DIRECTION('center_axis',(0.,0.,1.));
#4932=DIRECTION('ref_axis',(1.,0.,0.));
#4933=DIRECTION('',(0.,0.,1.));
#4934=DIRECTION('center_axis',(0.,0.,1.));
#4935=DIRECTION('ref_axis',(1.,0.,0.));
#4936=DIRECTION('',(0.,0.,-1.));
#4937=DIRECTION('center_axis',(0.,0.,1.));
#4938=DIRECTION('ref_axis',(-0.866025403784439,-0.5,0.));
#4939=DIRECTION('',(0.,0.,-1.));
#4940=DIRECTION('center_axis',(0.,0.,1.));
#4941=DIRECTION('ref_axis',(1.,0.,0.));
#4942=DIRECTION('',(0.,0.,1.));
#4943=DIRECTION('center_axis',(0.,0.,1.));
#4944=DIRECTION('ref_axis',(1.,0.,0.));
#4945=DIRECTION('center_axis',(0.,0.,1.));
#4946=DIRECTION('ref_axis',(1.,0.,0.));
#4947=DIRECTION('center_axis',(0.,0.,1.));
#4948=DIRECTION('ref_axis',(1.,0.,0.));
#4949=DIRECTION('center_axis',(0.,0.,1.));
#4950=DIRECTION('ref_axis',(1.,0.,0.));
#4951=DIRECTION('center_axis',(0.,0.,1.));
#4952=DIRECTION('ref_axis',(1.,0.,0.));
#4953=DIRECTION('center_axis',(0.,0.,1.));
#4954=DIRECTION('ref_axis',(1.,0.,0.));
#4955=DIRECTION('center_axis',(0.,0.,1.));
#4956=DIRECTION('ref_axis',(1.,0.,0.));
#4957=DIRECTION('',(0.,0.,1.));
#4958=DIRECTION('center_axis',(0.,0.,1.));
#4959=DIRECTION('ref_axis',(1.,0.,0.));
#4960=DIRECTION('',(0.,0.,-1.));
#4961=DIRECTION('center_axis',(0.,0.,1.));
#4962=DIRECTION('ref_axis',(1.,0.,0.));
#4963=DIRECTION('center_axis',(0.,0.,1.));
#4964=DIRECTION('ref_axis',(1.,0.,0.));
#4965=DIRECTION('center_axis',(0.,0.,1.));
#4966=DIRECTION('ref_axis',(1.,0.,0.));
#4967=DIRECTION('center_axis',(0.,0.,1.));
#4968=DIRECTION('ref_axis',(1.,0.,0.));
#4969=DIRECTION('',(0.,0.,1.));
#4970=DIRECTION('center_axis',(0.,0.,1.));
#4971=DIRECTION('ref_axis',(1.,0.,0.));
#4972=DIRECTION('',(0.,0.,-1.));
#4973=DIRECTION('center_axis',(0.,0.,1.));
#4974=DIRECTION('ref_axis',(1.,0.,0.));
#4975=DIRECTION('center_axis',(0.,0.,1.));
#4976=DIRECTION('ref_axis',(1.,0.,0.));
#4977=DIRECTION('center_axis',(0.,0.,1.));
#4978=DIRECTION('ref_axis',(1.,0.,0.));
#4979=DIRECTION('center_axis',(0.,0.,1.));
#4980=DIRECTION('ref_axis',(1.,0.,0.));
#4981=DIRECTION('',(0.,0.,1.));
#4982=DIRECTION('center_axis',(0.,0.,1.));
#4983=DIRECTION('ref_axis',(1.,0.,0.));
#4984=DIRECTION('',(0.,0.,-1.));
#4985=DIRECTION('center_axis',(0.,0.,1.));
#4986=DIRECTION('ref_axis',(-0.866025403784438,0.5,0.));
#4987=DIRECTION('',(0.,0.,-1.));
#4988=DIRECTION('center_axis',(0.,0.,1.));
#4989=DIRECTION('ref_axis',(1.,0.,0.));
#4990=DIRECTION('',(0.,0.,1.));
#4991=DIRECTION('center_axis',(0.,0.,1.));
#4992=DIRECTION('ref_axis',(1.,0.,0.));
#4993=DIRECTION('center_axis',(0.,0.,1.));
#4994=DIRECTION('ref_axis',(1.,0.,0.));
#4995=DIRECTION('center_axis',(0.,0.,1.));
#4996=DIRECTION('ref_axis',(1.,0.,0.));
#4997=DIRECTION('center_axis',(0.,0.,1.));
#4998=DIRECTION('ref_axis',(1.,0.,0.));
#4999=DIRECTION('center_axis',(0.,0.,1.));
#5000=DIRECTION('ref_axis',(1.,0.,0.));
#5001=DIRECTION('',(0.,0.,-1.));
#5002=DIRECTION('center_axis',(0.,0.,-1.));
#5003=DIRECTION('ref_axis',(1.,0.,0.));
#5004=DIRECTION('center_axis',(0.,0.,-1.));
#5005=DIRECTION('ref_axis',(1.,0.,0.));
#5006=DIRECTION('center_axis',(0.,0.,-1.));
#5007=DIRECTION('ref_axis',(1.,0.,0.));
#5008=DIRECTION('center_axis',(0.,0.,-1.));
#5009=DIRECTION('ref_axis',(1.,0.,0.));
#5010=DIRECTION('center_axis',(0.,0.,-1.));
#5011=DIRECTION('ref_axis',(1.,0.,0.));
#5012=DIRECTION('center_axis',(0.,0.,-1.));
#5013=DIRECTION('ref_axis',(1.,0.,0.));
#5014=DIRECTION('center_axis',(0.,0.,-1.));
#5015=DIRECTION('ref_axis',(1.,0.,0.));
#5016=DIRECTION('center_axis',(0.,0.,1.));
#5017=DIRECTION('ref_axis',(1.,0.,0.));
#5018=DIRECTION('center_axis',(0.,0.,1.));
#5019=DIRECTION('ref_axis',(1.,0.,0.));
#5020=DIRECTION('',(0.,0.,1.));
#5021=DIRECTION('center_axis',(0.,0.,-1.));
#5022=DIRECTION('ref_axis',(1.,0.,0.));
#5023=DIRECTION('center_axis',(0.,0.,1.));
#5024=DIRECTION('ref_axis',(1.,0.,0.));
#5025=DIRECTION('center_axis',(0.,0.,1.));
#5026=DIRECTION('ref_axis',(1.,0.,0.));
#5027=DIRECTION('',(0.,0.,1.));
#5028=DIRECTION('center_axis',(0.,0.,-1.));
#5029=DIRECTION('ref_axis',(1.,0.,0.));
#5030=DIRECTION('center_axis',(0.,0.,1.));
#5031=DIRECTION('ref_axis',(1.,0.,0.));
#5032=DIRECTION('center_axis',(0.,0.,1.));
#5033=DIRECTION('ref_axis',(1.,0.,0.));
#5034=DIRECTION('',(0.,0.,1.));
#5035=DIRECTION('center_axis',(0.,0.,-1.));
#5036=DIRECTION('ref_axis',(1.,0.,0.));
#5037=DIRECTION('center_axis',(0.,0.,1.));
#5038=DIRECTION('ref_axis',(1.,0.,0.));
#5039=DIRECTION('center_axis',(0.,0.,1.));
#5040=DIRECTION('ref_axis',(1.,0.,0.));
#5041=DIRECTION('',(0.,0.,1.));
#5042=DIRECTION('center_axis',(0.,0.,-1.));
#5043=DIRECTION('ref_axis',(1.,0.,0.));
#5044=DIRECTION('center_axis',(0.,0.,1.));
#5045=DIRECTION('ref_axis',(1.,0.,0.));
#5046=DIRECTION('center_axis',(0.,0.,1.));
#5047=DIRECTION('ref_axis',(1.,0.,0.));
#5048=DIRECTION('',(0.,0.,1.));
#5049=DIRECTION('center_axis',(0.,0.,-1.));
#5050=DIRECTION('ref_axis',(1.,0.,0.));
#5051=DIRECTION('center_axis',(0.,0.,1.));
#5052=DIRECTION('ref_axis',(1.,0.,0.));
#5053=DIRECTION('center_axis',(0.,0.,1.));
#5054=DIRECTION('ref_axis',(1.,0.,0.));
#5055=DIRECTION('',(0.,0.,1.));
#5056=DIRECTION('center_axis',(0.,0.,-1.));
#5057=DIRECTION('ref_axis',(1.,0.,0.));
#5058=DIRECTION('center_axis',(0.,0.,1.));
#5059=DIRECTION('ref_axis',(1.,0.,0.));
#5060=DIRECTION('center_axis',(0.,0.,1.));
#5061=DIRECTION('ref_axis',(1.,0.,0.));
#5062=DIRECTION('',(0.,0.,1.));
#5063=DIRECTION('center_axis',(0.,0.,-1.));
#5064=DIRECTION('ref_axis',(1.,0.,0.));
#5065=DIRECTION('center_axis',(0.,0.,1.));
#5066=DIRECTION('ref_axis',(1.,0.,0.));
#5067=DIRECTION('center_axis',(0.,0.,1.));
#5068=DIRECTION('ref_axis',(1.,0.,0.));
#5069=DIRECTION('',(0.,0.,1.));
#5070=DIRECTION('center_axis',(0.,0.,1.));
#5071=DIRECTION('ref_axis',(1.,0.,0.));
#5072=DIRECTION('center_axis',(0.,0.,1.));
#5073=DIRECTION('ref_axis',(1.,0.,0.));
#5074=DIRECTION('center_axis',(0.,0.,1.));
#5075=DIRECTION('ref_axis',(1.,0.,0.));
#5076=DIRECTION('center_axis',(0.,0.,1.));
#5077=DIRECTION('ref_axis',(1.,0.,0.));
#5078=DIRECTION('center_axis',(0.,0.,1.));
#5079=DIRECTION('ref_axis',(1.,0.,0.));
#5080=DIRECTION('',(0.,0.,-1.));
#5081=DIRECTION('center_axis',(0.,0.,1.));
#5082=DIRECTION('ref_axis',(1.,0.,0.));
#5083=DIRECTION('center_axis',(0.,0.,1.));
#5084=DIRECTION('ref_axis',(1.,0.,0.));
#5085=DIRECTION('center_axis',(0.,0.,1.));
#5086=DIRECTION('ref_axis',(1.,0.,0.));
#5087=DIRECTION('axis',(0.,0.,1.));
#5088=DIRECTION('refdir',(1.,0.,0.));
#5089=DIRECTION('center_axis',(-0.000134591856444243,0.997598919682403,
0.0692558830247305));
#5090=DIRECTION('ref_axis',(9.34371278597603E-6,-0.0692558823944232,0.997598928761687));
#5091=DIRECTION('center_axis',(0.000134591670588553,0.997598919668532,0.0692558832248945));
#5092=DIRECTION('ref_axis',(-0.499431472094232,0.0600671278230296,-0.864268560597272));
#5093=DIRECTION('center_axis',(0.000134591670588553,0.997598919668532,0.0692558832248945));
#5094=DIRECTION('ref_axis',(-0.499431472094232,0.0600671278230296,-0.864268560597272));
#5095=DIRECTION('center_axis',(-0.000134591856444243,0.997598919682403,
0.0692558830247305));
#5096=DIRECTION('ref_axis',(9.34371278597603E-6,-0.0692558823944232,0.997598928761687));
#5097=DIRECTION('axis',(0.,0.,1.));
#5098=DIRECTION('refdir',(1.,0.,0.));
#5099=DIRECTION('center_axis',(0.,0.,1.));
#5100=DIRECTION('ref_axis',(1.,0.,0.));
#5101=DIRECTION('center_axis',(0.,0.,1.));
#5102=DIRECTION('ref_axis',(1.,0.,0.));
#5103=DIRECTION('',(0.,0.,-1.));
#5104=DIRECTION('center_axis',(0.,0.,1.));
#5105=DIRECTION('ref_axis',(1.,0.,0.));
#5106=DIRECTION('center_axis',(0.,0.,1.));
#5107=DIRECTION('ref_axis',(1.,0.,0.));
#5108=DIRECTION('center_axis',(0.,0.,1.));
#5109=DIRECTION('ref_axis',(1.,0.,0.));
#5110=DIRECTION('center_axis',(0.,0.,1.));
#5111=DIRECTION('ref_axis',(1.,0.,0.));
#5112=DIRECTION('',(0.,0.,-1.));
#5113=DIRECTION('center_axis',(0.,0.,1.));
#5114=DIRECTION('ref_axis',(1.,0.,0.));
#5115=DIRECTION('center_axis',(0.,0.,1.));
#5116=DIRECTION('ref_axis',(1.,0.,0.));
#5117=DIRECTION('center_axis',(0.,0.,1.));
#5118=DIRECTION('ref_axis',(1.,0.,0.));
#5119=DIRECTION('axis',(0.,0.,1.));
#5120=DIRECTION('refdir',(1.,0.,0.));
#5121=DIRECTION('center_axis',(0.,0.,1.));
#5122=DIRECTION('ref_axis',(1.,0.,0.));
#5123=DIRECTION('center_axis',(0.,0.,1.));
#5124=DIRECTION('ref_axis',(1.,0.,0.));
#5125=DIRECTION('',(0.,0.,-1.));
#5126=DIRECTION('center_axis',(0.,0.,1.));
#5127=DIRECTION('ref_axis',(1.,0.,0.));
#5128=DIRECTION('center_axis',(0.,0.,1.));
#5129=DIRECTION('ref_axis',(1.,0.,0.));
#5130=DIRECTION('center_axis',(0.,0.,1.));
#5131=DIRECTION('ref_axis',(1.,0.,0.));
#5132=DIRECTION('axis',(0.,0.,1.));
#5133=DIRECTION('refdir',(1.,0.,0.));
#5134=DIRECTION('center_axis',(0.,1.,0.));
#5135=DIRECTION('ref_axis',(1.,0.,0.));
#5136=DIRECTION('',(0.,0.,1.));
#5137=DIRECTION('center_axis',(0.,1.,0.));
#5138=DIRECTION('ref_axis',(1.,0.,0.));
#5139=DIRECTION('center_axis',(0.,1.,0.));
#5140=DIRECTION('ref_axis',(1.,0.,0.));
#5141=DIRECTION('center_axis',(0.,1.,0.));
#5142=DIRECTION('ref_axis',(1.,0.,0.));
#5143=DIRECTION('center_axis',(0.,1.,0.));
#5144=DIRECTION('ref_axis',(1.,0.,0.));
#5145=DIRECTION('',(0.,1.,0.));
#5146=DIRECTION('center_axis',(0.,1.,0.));
#5147=DIRECTION('ref_axis',(1.,0.,0.));
#5148=DIRECTION('',(0.,0.,-1.));
#5149=DIRECTION('center_axis',(0.,0.,1.));
#5150=DIRECTION('ref_axis',(1.,0.,0.));
#5151=DIRECTION('center_axis',(0.,0.,-1.));
#5152=DIRECTION('ref_axis',(1.,0.,0.));
#5153=DIRECTION('',(0.,0.,-1.));
#5154=DIRECTION('center_axis',(0.,0.,-1.));
#5155=DIRECTION('ref_axis',(1.,0.,0.));
#5156=DIRECTION('center_axis',(0.,0.,1.));
#5157=DIRECTION('ref_axis',(1.,0.,0.));
#5158=DIRECTION('center_axis',(0.,0.,1.));
#5159=DIRECTION('ref_axis',(1.,0.,0.));
#5160=DIRECTION('',(0.,0.,-1.));
#5161=DIRECTION('center_axis',(0.,0.,1.));
#5162=DIRECTION('ref_axis',(1.,0.,0.));
#5163=DIRECTION('center_axis',(0.,0.,1.));
#5164=DIRECTION('ref_axis',(1.,0.,0.));
#5165=DIRECTION('center_axis',(0.,0.,1.));
#5166=DIRECTION('ref_axis',(1.,0.,0.));
#5167=DIRECTION('axis',(0.,0.,1.));
#5168=DIRECTION('refdir',(1.,0.,0.));
#5169=DIRECTION('center_axis',(0.,1.,0.));
#5170=DIRECTION('ref_axis',(-1.,0.,0.));
#5171=DIRECTION('',(-1.,0.,0.));
#5172=DIRECTION('',(0.,0.,1.));
#5173=DIRECTION('',(-1.,0.,0.));
#5174=DIRECTION('',(0.,0.,1.));
#5175=DIRECTION('center_axis',(1.,0.,0.));
#5176=DIRECTION('ref_axis',(0.,1.,0.));
#5177=DIRECTION('',(0.,1.,0.));
#5178=DIRECTION('',(0.,1.,0.));
#5179=DIRECTION('',(0.,0.,1.));
#5180=DIRECTION('center_axis',(0.,-1.,0.));
#5181=DIRECTION('ref_axis',(1.,0.,0.));
#5182=DIRECTION('',(1.,0.,0.));
#5183=DIRECTION('',(1.,0.,0.));
#5184=DIRECTION('',(0.,0.,1.));
#5185=DIRECTION('center_axis',(-1.,0.,0.));
#5186=DIRECTION('ref_axis',(0.,-1.,0.));
#5187=DIRECTION('',(0.,-1.,0.));
#5188=DIRECTION('',(0.,-1.,0.));
#5189=DIRECTION('center_axis',(0.,0.,1.));
#5190=DIRECTION('ref_axis',(1.,0.,0.));
#5191=DIRECTION('center_axis',(0.,0.,1.));
#5192=DIRECTION('ref_axis',(1.,0.,0.));
#5193=DIRECTION('axis',(0.,0.,1.));
#5194=DIRECTION('refdir',(1.,0.,0.));
#5195=DIRECTION('center_axis',(0.,1.,0.));
#5196=DIRECTION('ref_axis',(-1.,0.,0.));
#5197=DIRECTION('',(-1.,0.,0.));
#5198=DIRECTION('',(0.,0.,1.));
#5199=DIRECTION('',(-1.,0.,0.));
#5200=DIRECTION('',(0.,0.,1.));
#5201=DIRECTION('center_axis',(1.,0.,0.));
#5202=DIRECTION('ref_axis',(0.,1.,0.));
#5203=DIRECTION('',(0.,1.,0.));
#5204=DIRECTION('',(0.,1.,0.));
#5205=DIRECTION('',(0.,0.,1.));
#5206=DIRECTION('center_axis',(0.,-1.,0.));
#5207=DIRECTION('ref_axis',(1.,0.,0.));
#5208=DIRECTION('',(1.,0.,0.));
#5209=DIRECTION('',(1.,0.,0.));
#5210=DIRECTION('',(0.,0.,1.));
#5211=DIRECTION('center_axis',(-1.,0.,0.));
#5212=DIRECTION('ref_axis',(0.,-1.,0.));
#5213=DIRECTION('',(0.,-1.,0.));
#5214=DIRECTION('',(0.,-1.,0.));
#5215=DIRECTION('center_axis',(0.,0.,1.));
#5216=DIRECTION('ref_axis',(1.,0.,0.));
#5217=DIRECTION('center_axis',(0.,0.,1.));
#5218=DIRECTION('ref_axis',(1.,0.,0.));
#5219=DIRECTION('axis',(0.,0.,1.));
#5220=DIRECTION('refdir',(1.,0.,0.));
#5221=DIRECTION('center_axis',(0.,1.,0.));
#5222=DIRECTION('ref_axis',(0.,0.,1.));
#5223=DIRECTION('center_axis',(0.,-1.,0.));
#5224=DIRECTION('ref_axis',(1.,0.,0.));
#5225=DIRECTION('center_axis',(0.,-1.,0.));
#5226=DIRECTION('ref_axis',(1.,0.,0.));
#5227=DIRECTION('center_axis',(0.,-1.,0.));
#5228=DIRECTION('ref_axis',(1.,0.,0.));
#5229=DIRECTION('',(0.707106781186547,0.707106781186548,8.65956056235493E-17));
#5230=DIRECTION('center_axis',(0.,-1.,0.));
#5231=DIRECTION('ref_axis',(1.,0.,0.));
#5232=DIRECTION('center_axis',(0.,-1.,0.));
#5233=DIRECTION('ref_axis',(1.,0.,0.));
#5234=DIRECTION('',(0.,1.,0.));
#5235=DIRECTION('center_axis',(0.,1.,0.));
#5236=DIRECTION('ref_axis',(1.,0.,0.));
#5237=DIRECTION('center_axis',(0.,-1.,0.));
#5238=DIRECTION('ref_axis',(1.,0.,0.));
#5239=DIRECTION('',(-0.707106781186547,0.707106781186548,-8.65956056235493E-17));
#5240=DIRECTION('center_axis',(0.,-1.,0.));
#5241=DIRECTION('ref_axis',(0.,0.,-1.));
#5242=DIRECTION('center_axis',(0.,-1.,0.));
#5243=DIRECTION('ref_axis',(1.,0.,0.));
#5244=DIRECTION('center_axis',(0.,1.,0.));
#5245=DIRECTION('ref_axis',(1.,0.,0.));
#5246=DIRECTION('center_axis',(0.,1.,0.));
#5247=DIRECTION('ref_axis',(1.,0.,0.));
#5248=DIRECTION('',(-0.447213595499958,0.894427190999916,-5.47678698264203E-17));
#5249=DIRECTION('center_axis',(0.,-1.,0.));
#5250=DIRECTION('ref_axis',(1.,0.,0.));
#5251=DIRECTION('center_axis',(0.,1.,0.));
#5252=DIRECTION('ref_axis',(1.,0.,0.));
#5253=DIRECTION('',(0.,1.,0.));
#5254=DIRECTION('center_axis',(0.,1.,0.));
#5255=DIRECTION('ref_axis',(1.,0.,0.));
#5256=DIRECTION('center_axis',(0.,-1.,0.));
#5257=DIRECTION('ref_axis',(1.,0.,0.));
#5258=DIRECTION('',(-0.707106781186547,0.707106781186548,-8.65956056235493E-17));
#5259=DIRECTION('center_axis',(0.,-1.,0.));
#5260=DIRECTION('ref_axis',(0.,0.,-1.));
#5261=DIRECTION('center_axis',(0.866025403784439,0.,-0.5));
#5262=DIRECTION('ref_axis',(0.5,0.,0.866025403784439));
#5263=DIRECTION('',(-0.5,0.,-0.866025403784439));
#5264=DIRECTION('',(0.,-1.,0.));
#5265=DIRECTION('',(0.5,0.,0.866025403784439));
#5266=DIRECTION('',(0.,-1.,0.));
#5267=DIRECTION('center_axis',(1.60246890531964E-16,0.,-1.));
#5268=DIRECTION('ref_axis',(1.,0.,1.60246890531964E-16));
#5269=DIRECTION('',(-1.,0.,-1.60246890531964E-16));
#5270=DIRECTION('',(0.,-1.,0.));
#5271=DIRECTION('',(1.,0.,1.60246890531964E-16));
#5272=DIRECTION('center_axis',(-0.866025403784439,0.,-0.5));
#5273=DIRECTION('ref_axis',(0.5,0.,-0.866025403784439));
#5274=DIRECTION('',(-0.5,0.,0.866025403784439));
#5275=DIRECTION('',(0.,-1.,0.));
#5276=DIRECTION('',(0.5,0.,-0.866025403784439));
#5277=DIRECTION('center_axis',(-0.866025403784439,0.,0.5));
#5278=DIRECTION('ref_axis',(-0.5,0.,-0.866025403784439));
#5279=DIRECTION('',(0.5,0.,0.866025403784439));
#5280=DIRECTION('',(0.,-1.,0.));
#5281=DIRECTION('',(-0.5,0.,-0.866025403784439));
#5282=DIRECTION('center_axis',(-1.60246890531964E-16,0.,1.));
#5283=DIRECTION('ref_axis',(-1.,0.,-1.60246890531964E-16));
#5284=DIRECTION('',(1.,0.,1.60246890531964E-16));
#5285=DIRECTION('',(0.,-1.,0.));
#5286=DIRECTION('',(-1.,0.,-1.60246890531964E-16));
#5287=DIRECTION('center_axis',(0.866025403784439,0.,0.5));
#5288=DIRECTION('ref_axis',(-0.5,0.,0.866025403784439));
#5289=DIRECTION('',(0.5,0.,-0.866025403784439));
#5290=DIRECTION('',(-0.5,0.,0.866025403784439));
#5291=DIRECTION('center_axis',(0.,1.,0.));
#5292=DIRECTION('ref_axis',(1.,0.,0.));
#5293=DIRECTION('center_axis',(0.,-1.,0.));
#5294=DIRECTION('ref_axis',(0.,0.,-1.));
#5295=DIRECTION('axis',(0.,0.,1.));
#5296=DIRECTION('refdir',(1.,0.,0.));
#5297=DIRECTION('center_axis',(0.,1.,0.));
#5298=DIRECTION('ref_axis',(1.,0.,0.));
#5299=DIRECTION('',(-0.5,0.,0.866025403784439));
#5300=DIRECTION('',(-1.,0.,-3.29650746237182E-16));
#5301=DIRECTION('',(-0.5,0.,-0.866025403784439));
#5302=DIRECTION('',(0.5,0.,-0.866025403784438));
#5303=DIRECTION('',(1.,0.,0.));
#5304=DIRECTION('',(0.5,0.,0.866025403784439));
#5305=DIRECTION('center_axis',(0.,-1.,0.));
#5306=DIRECTION('ref_axis',(1.,0.,0.));
#5307=DIRECTION('center_axis',(0.,1.,0.));
#5308=DIRECTION('ref_axis',(1.,0.,0.));
#5309=DIRECTION('',(0.5,0.,-0.866025403784439));
#5310=DIRECTION('',(-0.5,0.,-0.866025403784439));
#5311=DIRECTION('',(-1.,0.,0.));
#5312=DIRECTION('',(-0.5,0.,0.866025403784438));
#5313=DIRECTION('',(0.5,0.,0.866025403784439));
#5314=DIRECTION('',(1.,0.,3.29650746237182E-16));
#5315=DIRECTION('center_axis',(0.,1.,0.));
#5316=DIRECTION('ref_axis',(1.,0.,0.));
#5317=DIRECTION('center_axis',(-3.29650746237182E-16,0.,1.));
#5318=DIRECTION('ref_axis',(1.,0.,3.29650746237182E-16));
#5319=DIRECTION('',(0.,-1.,0.));
#5320=DIRECTION('',(0.,1.,0.));
#5321=DIRECTION('center_axis',(-0.866025403784439,0.,0.5));
#5322=DIRECTION('ref_axis',(0.5,0.,0.866025403784439));
#5323=DIRECTION('',(0.,1.,0.));
#5324=DIRECTION('center_axis',(-0.866025403784439,0.,-0.5));
#5325=DIRECTION('ref_axis',(-0.5,0.,0.866025403784439));
#5326=DIRECTION('',(0.,1.,0.));
#5327=DIRECTION('center_axis',(0.,0.,-1.));
#5328=DIRECTION('ref_axis',(-1.,0.,0.));
#5329=DIRECTION('',(0.,1.,0.));
#5330=DIRECTION('center_axis',(0.866025403784439,0.,-0.5));
#5331=DIRECTION('ref_axis',(-0.5,0.,-0.866025403784439));
#5332=DIRECTION('',(0.,1.,0.));
#5333=DIRECTION('center_axis',(0.866025403784439,0.,0.5));
#5334=DIRECTION('ref_axis',(0.5,0.,-0.866025403784439));
#5335=DIRECTION('center_axis',(0.,-1.,0.));
#5336=DIRECTION('ref_axis',(1.,0.,0.));
#5337=DIRECTION('',(0.,1.,0.));
#5338=DIRECTION('center_axis',(0.,-1.,0.));
#5339=DIRECTION('ref_axis',(1.,0.,0.));
#5340=DIRECTION('center_axis',(0.,1.,0.));
#5341=DIRECTION('ref_axis',(0.,0.,1.));
#5342=DIRECTION('center_axis',(0.,-1.,0.));
#5343=DIRECTION('ref_axis',(1.,0.,0.));
#5344=DIRECTION('center_axis',(0.,-1.,0.));
#5345=DIRECTION('ref_axis',(1.,0.,0.));
#5346=DIRECTION('center_axis',(0.,-1.,0.));
#5347=DIRECTION('ref_axis',(1.,0.,0.));
#5348=DIRECTION('',(0.707106781186547,0.707106781186548,8.65956056235493E-17));
#5349=DIRECTION('center_axis',(0.,-1.,0.));
#5350=DIRECTION('ref_axis',(1.,0.,0.));
#5351=DIRECTION('center_axis',(0.,-1.,0.));
#5352=DIRECTION('ref_axis',(1.,0.,0.));
#5353=DIRECTION('',(0.,1.,0.));
#5354=DIRECTION('center_axis',(0.,1.,0.));
#5355=DIRECTION('ref_axis',(1.,0.,0.));
#5356=DIRECTION('center_axis',(0.,-1.,0.));
#5357=DIRECTION('ref_axis',(1.,0.,0.));
#5358=DIRECTION('',(-0.707106781186547,0.707106781186548,-8.65956056235493E-17));
#5359=DIRECTION('center_axis',(0.,-1.,0.));
#5360=DIRECTION('ref_axis',(0.,0.,-1.));
#5361=DIRECTION('center_axis',(0.,-1.,0.));
#5362=DIRECTION('ref_axis',(1.,0.,0.));
#5363=DIRECTION('center_axis',(0.,-1.,0.));
#5364=DIRECTION('ref_axis',(1.,0.,0.));
#5365=DIRECTION('',(0.,1.,0.));
#5366=DIRECTION('axis',(0.,0.,1.));
#5367=DIRECTION('refdir',(1.,0.,0.));
#5368=DIRECTION('center_axis',(0.,1.,0.));
#5369=DIRECTION('ref_axis',(0.,0.,1.));
#5370=DIRECTION('center_axis',(0.,-1.,0.));
#5371=DIRECTION('ref_axis',(1.,0.,0.));
#5372=DIRECTION('center_axis',(0.,-1.,0.));
#5373=DIRECTION('ref_axis',(1.,0.,0.));
#5374=DIRECTION('center_axis',(0.,-1.,0.));
#5375=DIRECTION('ref_axis',(1.,0.,0.));
#5376=DIRECTION('',(0.707106781186548,0.707106781186547,8.65956056235493E-17));
#5377=DIRECTION('center_axis',(0.,-1.,0.));
#5378=DIRECTION('ref_axis',(1.,0.,0.));
#5379=DIRECTION('center_axis',(0.,-1.,0.));
#5380=DIRECTION('ref_axis',(1.,0.,0.));
#5381=DIRECTION('',(0.,1.,0.));
#5382=DIRECTION('center_axis',(0.,1.,0.));
#5383=DIRECTION('ref_axis',(1.,0.,0.));
#5384=DIRECTION('center_axis',(0.,-1.,0.));
#5385=DIRECTION('ref_axis',(1.,0.,0.));
#5386=DIRECTION('',(-0.707106781186547,0.707106781186548,-8.65956056235493E-17));
#5387=DIRECTION('center_axis',(0.,-1.,0.));
#5388=DIRECTION('ref_axis',(0.,0.,-1.));
#5389=DIRECTION('center_axis',(0.,-1.,0.));
#5390=DIRECTION('ref_axis',(1.,0.,0.));
#5391=DIRECTION('center_axis',(0.,1.,0.));
#5392=DIRECTION('ref_axis',(1.,0.,0.));
#5393=DIRECTION('center_axis',(0.,1.,0.));
#5394=DIRECTION('ref_axis',(1.,0.,0.));
#5395=DIRECTION('',(-0.447213595499958,0.894427190999916,-5.47678698264203E-17));
#5396=DIRECTION('center_axis',(0.,-1.,0.));
#5397=DIRECTION('ref_axis',(1.,0.,0.));
#5398=DIRECTION('center_axis',(0.,1.,0.));
#5399=DIRECTION('ref_axis',(1.,0.,0.));
#5400=DIRECTION('',(0.,1.,0.));
#5401=DIRECTION('center_axis',(0.,1.,0.));
#5402=DIRECTION('ref_axis',(1.,0.,0.));
#5403=DIRECTION('center_axis',(0.,-1.,0.));
#5404=DIRECTION('ref_axis',(1.,0.,0.));
#5405=DIRECTION('',(-0.707106781186547,0.707106781186548,-8.65956056235493E-17));
#5406=DIRECTION('center_axis',(0.,-1.,0.));
#5407=DIRECTION('ref_axis',(0.,0.,-1.));
#5408=DIRECTION('center_axis',(0.866025403784439,0.,-0.5));
#5409=DIRECTION('ref_axis',(0.5,0.,0.866025403784439));
#5410=DIRECTION('',(-0.5,0.,-0.866025403784439));
#5411=DIRECTION('',(0.,-1.,0.));
#5412=DIRECTION('',(0.5,0.,0.866025403784439));
#5413=DIRECTION('',(0.,-1.,0.));
#5414=DIRECTION('center_axis',(1.20185167898973E-16,0.,-1.));
#5415=DIRECTION('ref_axis',(1.,0.,1.20185167898973E-16));
#5416=DIRECTION('',(-1.,0.,-1.20185167898973E-16));
#5417=DIRECTION('',(0.,-1.,0.));
#5418=DIRECTION('',(1.,0.,1.20185167898973E-16));
#5419=DIRECTION('center_axis',(-0.866025403784439,0.,-0.5));
#5420=DIRECTION('ref_axis',(0.5,0.,-0.866025403784439));
#5421=DIRECTION('',(-0.5,0.,0.866025403784439));
#5422=DIRECTION('',(0.,-1.,0.));
#5423=DIRECTION('',(0.5,0.,-0.866025403784439));
#5424=DIRECTION('center_axis',(-0.866025403784439,0.,0.5));
#5425=DIRECTION('ref_axis',(-0.5,0.,-0.866025403784439));
#5426=DIRECTION('',(0.5,0.,0.866025403784439));
#5427=DIRECTION('',(0.,-1.,0.));
#5428=DIRECTION('',(-0.5,0.,-0.866025403784439));
#5429=DIRECTION('center_axis',(-2.40370335797945E-16,0.,1.));
#5430=DIRECTION('ref_axis',(-1.,0.,-2.40370335797945E-16));
#5431=DIRECTION('',(1.,0.,2.40370335797945E-16));
#5432=DIRECTION('',(0.,-1.,0.));
#5433=DIRECTION('',(-1.,0.,-2.40370335797945E-16));
#5434=DIRECTION('center_axis',(0.866025403784439,0.,0.5));
#5435=DIRECTION('ref_axis',(-0.5,0.,0.866025403784439));
#5436=DIRECTION('',(0.5,0.,-0.866025403784439));
#5437=DIRECTION('',(-0.5,0.,0.866025403784439));
#5438=DIRECTION('center_axis',(0.,1.,0.));
#5439=DIRECTION('ref_axis',(1.,0.,0.));
#5440=DIRECTION('center_axis',(0.,-1.,0.));
#5441=DIRECTION('ref_axis',(0.,0.,-1.));
#5442=DIRECTION('axis',(0.,0.,1.));
#5443=DIRECTION('refdir',(1.,0.,0.));
#5444=DIRECTION('center_axis',(0.,1.,0.));
#5445=DIRECTION('ref_axis',(1.,0.,0.));
#5446=DIRECTION('center_axis',(0.,-1.,0.));
#5447=DIRECTION('ref_axis',(1.,0.,0.));
#5448=DIRECTION('',(0.,-1.,0.));
#5449=DIRECTION('center_axis',(0.,-1.,0.));
#5450=DIRECTION('ref_axis',(1.,0.,0.));
#5451=DIRECTION('center_axis',(0.,1.,0.));
#5452=DIRECTION('ref_axis',(1.,0.,0.));
#5453=DIRECTION('center_axis',(0.,1.,0.));
#5454=DIRECTION('ref_axis',(1.,0.,0.));
#5455=DIRECTION('',(0.,-1.,0.));
#5456=DIRECTION('center_axis',(0.,1.,0.));
#5457=DIRECTION('ref_axis',(1.,0.,0.));
#5458=DIRECTION('center_axis',(0.,1.,0.));
#5459=DIRECTION('ref_axis',(1.,0.,0.));
#5460=DIRECTION('center_axis',(0.,1.,0.));
#5461=DIRECTION('ref_axis',(1.,0.,0.));
#5462=DIRECTION('axis',(0.,0.,1.));
#5463=DIRECTION('refdir',(1.,0.,0.));
#5464=DIRECTION('center_axis',(0.,1.,0.));
#5465=DIRECTION('ref_axis',(1.,0.,0.));
#5466=DIRECTION('',(0.866025403784439,-0.5,1.06057523872491E-16));
#5467=DIRECTION('center_axis',(0.,-1.,0.));
#5468=DIRECTION('ref_axis',(1.,0.,0.));
#5469=DIRECTION('center_axis',(0.,-1.,0.));
#5470=DIRECTION('ref_axis',(1.,0.,0.));
#5471=DIRECTION('center_axis',(0.,1.,0.));
#5472=DIRECTION('ref_axis',(1.,0.,0.));
#5473=DIRECTION('',(-0.866025403784439,-0.5,-1.06057523872491E-16));
#5474=DIRECTION('center_axis',(1.4792020664489E-16,0.,-1.));
#5475=DIRECTION('ref_axis',(-1.,0.,-1.4792020664489E-16));
#5476=DIRECTION('',(0.,1.,0.));
#5477=DIRECTION('',(0.,1.,0.));
#5478=DIRECTION('center_axis',(-0.866025403784439,0.,-0.5));
#5479=DIRECTION('ref_axis',(-0.5,0.,0.866025403784439));
#5480=DIRECTION('',(0.,1.,0.));
#5481=DIRECTION('center_axis',(-0.866025403784439,0.,0.5));
#5482=DIRECTION('ref_axis',(0.5,0.,0.866025403784439));
#5483=DIRECTION('',(0.,1.,0.));
#5484=DIRECTION('center_axis',(0.,1.,0.));
#5485=DIRECTION('ref_axis',(1.,0.,0.));
#5486=DIRECTION('center_axis',(0.,1.,0.));
#5487=DIRECTION('ref_axis',(1.,0.,0.));
#5488=DIRECTION('',(0.,-1.,0.));
#5489=DIRECTION('center_axis',(0.,1.,0.));
#5490=DIRECTION('ref_axis',(1.,0.,0.));
#5491=DIRECTION('center_axis',(-2.95840413289779E-16,0.,1.));
#5492=DIRECTION('ref_axis',(1.,0.,2.95840413289779E-16));
#5493=DIRECTION('',(0.,1.,0.));
#5494=DIRECTION('center_axis',(0.866025403784439,0.,-0.5));
#5495=DIRECTION('ref_axis',(-0.5,0.,-0.866025403784439));
#5496=DIRECTION('',(0.,1.,0.));
#5497=DIRECTION('center_axis',(0.866025403784439,0.,0.5));
#5498=DIRECTION('ref_axis',(0.5,0.,-0.866025403784439));
#5499=DIRECTION('center_axis',(0.,1.,0.));
#5500=DIRECTION('ref_axis',(1.,0.,0.));
#5501=DIRECTION('center_axis',(0.,1.,0.));
#5502=DIRECTION('ref_axis',(1.,0.,0.));
#5503=DIRECTION('axis',(0.,0.,1.));
#5504=DIRECTION('refdir',(1.,0.,0.));
#5505=DIRECTION('center_axis',(0.866025403784439,0.,-0.5));
#5506=DIRECTION('ref_axis',(0.5,0.,0.866025403784439));
#5507=DIRECTION('',(0.5,0.,0.866025403784439));
#5508=DIRECTION('',(0.,-1.,0.));
#5509=DIRECTION('',(0.5,0.,0.866025403784439));
#5510=DIRECTION('',(0.,-1.,0.));
#5511=DIRECTION('center_axis',(1.20185167898973E-16,0.,-1.));
#5512=DIRECTION('ref_axis',(1.,0.,1.20185167898973E-16));
#5513=DIRECTION('',(1.,0.,1.20185167898973E-16));
#5514=DIRECTION('',(0.,-1.,0.));
#5515=DIRECTION('',(1.,0.,1.20185167898973E-16));
#5516=DIRECTION('center_axis',(-0.866025403784439,0.,-0.5));
#5517=DIRECTION('ref_axis',(0.5,0.,-0.866025403784439));
#5518=DIRECTION('',(0.5,0.,-0.866025403784439));
#5519=DIRECTION('',(0.,-1.,0.));
#5520=DIRECTION('',(0.5,0.,-0.866025403784439));
#5521=DIRECTION('center_axis',(-0.866025403784439,0.,0.5));
#5522=DIRECTION('ref_axis',(-0.5,0.,-0.866025403784439));
#5523=DIRECTION('',(-0.5,0.,-0.866025403784439));
#5524=DIRECTION('',(0.,-1.,0.));
#5525=DIRECTION('',(-0.5,0.,-0.866025403784439));
#5526=DIRECTION('center_axis',(-2.40370335797945E-16,0.,1.));
#5527=DIRECTION('ref_axis',(-1.,0.,-2.40370335797945E-16));
#5528=DIRECTION('',(-1.,0.,-2.40370335797945E-16));
#5529=DIRECTION('',(0.,-1.,0.));
#5530=DIRECTION('',(-1.,0.,-2.40370335797945E-16));
#5531=DIRECTION('center_axis',(0.866025403784439,0.,0.5));
#5532=DIRECTION('ref_axis',(-0.5,0.,0.866025403784439));
#5533=DIRECTION('',(-0.5,0.,0.866025403784439));
#5534=DIRECTION('',(-0.5,0.,0.866025403784439));
#5535=DIRECTION('center_axis',(0.,-1.,0.));
#5536=DIRECTION('ref_axis',(0.,0.,-1.));
#5537=DIRECTION('center_axis',(0.,1.,0.));
#5538=DIRECTION('ref_axis',(0.,0.,1.));
#5539=DIRECTION('center_axis',(0.,-1.,0.));
#5540=DIRECTION('ref_axis',(1.,0.,0.));
#5541=DIRECTION('center_axis',(0.,-1.,0.));
#5542=DIRECTION('ref_axis',(1.,0.,0.));
#5543=DIRECTION('center_axis',(0.,-1.,0.));
#5544=DIRECTION('ref_axis',(1.,0.,0.));
#5545=DIRECTION('',(0.707106781186548,0.707106781186547,8.65956056235494E-17));
#5546=DIRECTION('center_axis',(0.,-1.,0.));
#5547=DIRECTION('ref_axis',(1.,0.,0.));
#5548=DIRECTION('center_axis',(0.,1.,0.));
#5549=DIRECTION('ref_axis',(1.,0.,0.));
#5550=DIRECTION('',(0.,1.,0.));
#5551=DIRECTION('center_axis',(0.,1.,0.));
#5552=DIRECTION('ref_axis',(1.,0.,0.));
#5553=DIRECTION('center_axis',(0.,-1.,0.));
#5554=DIRECTION('ref_axis',(1.,0.,0.));
#5555=DIRECTION('',(-0.707106781186548,0.707106781186547,-8.65956056235494E-17));
#5556=DIRECTION('center_axis',(0.,-1.,0.));
#5557=DIRECTION('ref_axis',(0.,0.,-1.));
#5558=DIRECTION('',(0.,0.,1.));
#5559=DIRECTION('',(1.,0.,0.));
#5560=DIRECTION('',(0.,0.,1.));
#5561=DIRECTION('',(1.,0.,0.));
#5562=DIRECTION('',(0.,0.,1.));
#5563=DIRECTION('',(1.,0.,0.));
#5564=DIRECTION('',(0.,0.,1.));
#5565=DIRECTION('',(1.,0.,0.));
#5566=DIRECTION('',(0.,0.,1.));
#5567=DIRECTION('',(1.,0.,0.));
#5568=DIRECTION('',(0.,0.,1.));
#5569=DIRECTION('',(1.,0.,0.));
#5570=DIRECTION('',(0.,0.,1.));
#5571=DIRECTION('',(1.,0.,0.));
#5572=DIRECTION('',(0.,0.,1.));
#5573=DIRECTION('',(1.,0.,0.));
#5574=DIRECTION('',(0.,0.,1.));
#5575=DIRECTION('',(1.,0.,0.));
#5576=DIRECTION('',(0.,0.,1.));
#5577=DIRECTION('',(1.,0.,0.));
#5578=DIRECTION('',(0.,0.,1.));
#5579=DIRECTION('',(1.,0.,0.));
#5580=DIRECTION('',(0.,0.,1.));
#5581=DIRECTION('',(1.,0.,0.));
#5582=DIRECTION('',(0.,0.,1.));
#5583=DIRECTION('',(1.,0.,0.));
#5584=DIRECTION('',(0.,0.,1.));
#5585=DIRECTION('',(1.,0.,0.));
#5586=DIRECTION('',(0.,0.,1.));
#5587=DIRECTION('',(1.,0.,0.));
#5588=DIRECTION('',(0.,0.,1.));
#5589=DIRECTION('',(1.,0.,0.));
#5590=DIRECTION('',(0.,0.,1.));
#5591=DIRECTION('',(1.,0.,0.));
#5592=DIRECTION('',(0.,0.,1.));
#5593=DIRECTION('',(1.,0.,0.));
#5594=DIRECTION('',(0.,1.,2.22044604925031E-16));
#5595=DIRECTION('',(1.,0.,0.));
#5596=DIRECTION('',(0.,1.,2.22044604925031E-16));
#5597=DIRECTION('',(1.,0.,0.));
#5598=DIRECTION('',(0.,0.,1.));
#5599=DIRECTION('',(2.22044604925031E-16,-1.,0.));
#5600=DIRECTION('',(0.,0.,1.));
#5601=DIRECTION('',(2.22044604925031E-16,-1.,0.));
#5602=DIRECTION('',(0.,-1.,2.22044604925031E-16));
#5603=DIRECTION('',(1.,0.,0.));
#5604=DIRECTION('',(0.,-1.,2.22044604925031E-16));
#5605=DIRECTION('',(1.,0.,0.));
#5606=DIRECTION('',(0.,-1.,2.22044604925031E-16));
#5607=DIRECTION('',(1.,0.,0.));
#5608=DIRECTION('',(0.,-1.,2.22044604925031E-16));
#5609=DIRECTION('',(1.,0.,0.));
#5610=DIRECTION('',(0.,-1.,2.22044604925031E-16));
#5611=DIRECTION('',(1.,0.,0.));
#5612=DIRECTION('',(0.,-1.,2.22044604925031E-16));
#5613=DIRECTION('',(1.,0.,0.));
#5614=DIRECTION('',(0.,-1.,2.22044604925031E-16));
#5615=DIRECTION('',(1.,0.,0.));
#5616=DIRECTION('',(0.,-1.,2.22044604925031E-16));
#5617=DIRECTION('',(1.,0.,0.));
#5618=DIRECTION('',(0.,0.,1.));
#5619=DIRECTION('',(1.,0.,0.));
#5620=CARTESIAN_POINT('',(0.,0.,0.));
#5621=CARTESIAN_POINT('',(0.,0.,0.));
#5622=CARTESIAN_POINT('Origin',(0.,-3.,-0.1));
#5623=CARTESIAN_POINT('',(-0.225,-3.,0.));
#5624=CARTESIAN_POINT('Origin',(0.,-3.,0.));
#5625=CARTESIAN_POINT('',(-0.225,-3.,0.6));
#5626=CARTESIAN_POINT('',(-0.225,-3.,-0.1));
#5627=CARTESIAN_POINT('Origin',(0.,-3.,0.6));
#5628=CARTESIAN_POINT('Origin',(0.,3.,-0.1));
#5629=CARTESIAN_POINT('',(-0.225,3.,0.));
#5630=CARTESIAN_POINT('Origin',(0.,3.,0.));
#5631=CARTESIAN_POINT('',(-0.225,3.,0.6));
#5632=CARTESIAN_POINT('',(-0.225,3.,-0.1));
#5633=CARTESIAN_POINT('Origin',(0.,3.,0.6));
#5634=CARTESIAN_POINT('Origin',(6.,4.5,0.));
#5635=CARTESIAN_POINT('',(6.,4.5,0.));
#5636=CARTESIAN_POINT('',(-6.,4.5,0.));
#5637=CARTESIAN_POINT('',(6.,4.5,0.));
#5638=CARTESIAN_POINT('',(-6.,4.5,0.6));
#5639=CARTESIAN_POINT('',(-6.,4.5,0.));
#5640=CARTESIAN_POINT('',(6.,4.5,0.6));
#5641=CARTESIAN_POINT('',(6.,4.5,0.6));
#5642=CARTESIAN_POINT('',(6.,4.5,0.));
#5643=CARTESIAN_POINT('Origin',(6.,-4.5,0.));
#5644=CARTESIAN_POINT('',(6.,-4.5,0.));
#5645=CARTESIAN_POINT('',(6.,-4.5,0.));
#5646=CARTESIAN_POINT('',(6.,-4.5,0.6));
#5647=CARTESIAN_POINT('',(6.,-4.5,0.6));
#5648=CARTESIAN_POINT('',(6.,-4.5,0.));
#5649=CARTESIAN_POINT('Origin',(-6.,-4.5,0.));
#5650=CARTESIAN_POINT('',(-6.,-4.5,0.));
#5651=CARTESIAN_POINT('',(-6.,-4.5,0.));
#5652=CARTESIAN_POINT('',(-6.,-4.5,0.6));
#5653=CARTESIAN_POINT('',(-6.,-4.5,0.6));
#5654=CARTESIAN_POINT('',(-6.,-4.5,0.));
#5655=CARTESIAN_POINT('Origin',(-6.,4.5,0.));
#5656=CARTESIAN_POINT('',(-6.,4.5,0.));
#5657=CARTESIAN_POINT('',(-6.,4.5,0.6));
#5658=CARTESIAN_POINT('Origin',(0.,0.,0.6));
#5659=CARTESIAN_POINT('Origin',(0.,0.,0.));
#5660=CARTESIAN_POINT('',(0.,0.,0.));
#5661=CARTESIAN_POINT('Origin',(0.,-3.,0.5));
#5662=CARTESIAN_POINT('',(-0.225,-3.,0.6));
#5663=CARTESIAN_POINT('Origin',(0.,-3.,0.6));
#5664=CARTESIAN_POINT('',(-0.225,-3.,1.));
#5665=CARTESIAN_POINT('',(-0.225,-3.,0.5));
#5666=CARTESIAN_POINT('Origin',(0.,-3.,1.));
#5667=CARTESIAN_POINT('Origin',(1.,-2.2,0.6));
#5668=CARTESIAN_POINT('',(1.,-2.2,0.6));
#5669=CARTESIAN_POINT('',(-1.,-2.2,0.6));
#5670=CARTESIAN_POINT('',(1.,-2.2,0.6));
#5671=CARTESIAN_POINT('',(-1.,-2.2,1.));
#5672=CARTESIAN_POINT('',(-1.,-2.2,0.6));
#5673=CARTESIAN_POINT('',(1.,-2.2,1.));
#5674=CARTESIAN_POINT('',(1.,-2.2,1.));
#5675=CARTESIAN_POINT('',(1.,-2.2,0.6));
#5676=CARTESIAN_POINT('Origin',(1.,-3.8,0.6));
#5677=CARTESIAN_POINT('',(1.,-3.8,0.6));
#5678=CARTESIAN_POINT('',(1.,-3.8,0.6));
#5679=CARTESIAN_POINT('',(1.,-3.8,1.));
#5680=CARTESIAN_POINT('',(1.,-3.8,1.));
#5681=CARTESIAN_POINT('',(1.,-3.8,0.6));
#5682=CARTESIAN_POINT('Origin',(-1.,-3.8,0.6));
#5683=CARTESIAN_POINT('',(-1.,-3.8,0.6));
#5684=CARTESIAN_POINT('',(-1.,-3.8,0.6));
#5685=CARTESIAN_POINT('',(-1.,-3.8,1.));
#5686=CARTESIAN_POINT('',(-1.,-3.8,1.));
#5687=CARTESIAN_POINT('',(-1.,-3.8,0.6));
#5688=CARTESIAN_POINT('Origin',(-1.,-2.2,0.6));
#5689=CARTESIAN_POINT('',(-1.,-2.2,0.6));
#5690=CARTESIAN_POINT('',(-1.,-2.2,1.));
#5691=CARTESIAN_POINT('Origin',(0.,-3.,1.));
#5692=CARTESIAN_POINT('Origin',(0.,-3.,0.6));
#5693=CARTESIAN_POINT('',(0.,0.,0.));
#5694=CARTESIAN_POINT('Origin',(0.,3.,0.5));
#5695=CARTESIAN_POINT('',(-0.225,3.,0.6));
#5696=CARTESIAN_POINT('Origin',(0.,3.,0.6));
#5697=CARTESIAN_POINT('',(-0.225,3.,1.));
#5698=CARTESIAN_POINT('',(-0.225,3.,0.5));
#5699=CARTESIAN_POINT('Origin',(0.,3.,1.));
#5700=CARTESIAN_POINT('Origin',(1.,3.8,0.6));
#5701=CARTESIAN_POINT('',(1.,3.8,0.6));
#5702=CARTESIAN_POINT('',(-1.,3.8,0.6));
#5703=CARTESIAN_POINT('',(1.,3.8,0.6));
#5704=CARTESIAN_POINT('',(-1.,3.8,1.));
#5705=CARTESIAN_POINT('',(-1.,3.8,0.6));
#5706=CARTESIAN_POINT('',(1.,3.8,1.));
#5707=CARTESIAN_POINT('',(1.,3.8,1.));
#5708=CARTESIAN_POINT('',(1.,3.8,0.6));
#5709=CARTESIAN_POINT('Origin',(1.,2.2,0.6));
#5710=CARTESIAN_POINT('',(1.,2.2,0.6));
#5711=CARTESIAN_POINT('',(1.,2.2,0.6));
#5712=CARTESIAN_POINT('',(1.,2.2,1.));
#5713=CARTESIAN_POINT('',(1.,2.2,1.));
#5714=CARTESIAN_POINT('',(1.,2.2,0.6));
#5715=CARTESIAN_POINT('Origin',(-1.,2.2,0.6));
#5716=CARTESIAN_POINT('',(-1.,2.2,0.6));
#5717=CARTESIAN_POINT('',(-1.,2.2,0.6));
#5718=CARTESIAN_POINT('',(-1.,2.2,1.));
#5719=CARTESIAN_POINT('',(-1.,2.2,1.));
#5720=CARTESIAN_POINT('',(-1.,2.2,0.6));
#5721=CARTESIAN_POINT('Origin',(-1.,3.8,0.6));
#5722=CARTESIAN_POINT('',(-1.,3.8,0.6));
#5723=CARTESIAN_POINT('',(-1.,3.8,1.));
#5724=CARTESIAN_POINT('Origin',(0.,3.,1.));
#5725=CARTESIAN_POINT('Origin',(0.,3.,0.6));
#5726=CARTESIAN_POINT('',(0.,0.,0.));
#5727=CARTESIAN_POINT('Origin',(-6.2456986756515E-16,-3.4,3.5));
#5728=CARTESIAN_POINT('',(-0.210000000000001,-3.4,3.5));
#5729=CARTESIAN_POINT('Origin',(-6.2456986756515E-16,-3.4,3.5));
#5730=CARTESIAN_POINT('',(-0.210000000000001,-3.4,5.));
#5731=CARTESIAN_POINT('',(-0.210000000000001,-3.4,3.5));
#5732=CARTESIAN_POINT('Origin',(-6.2456986756515E-16,-3.4,5.));
#5733=CARTESIAN_POINT('Origin',(-6.38378239159465E-16,-3.4,3.5));
#5734=CARTESIAN_POINT('Origin',(2.94448637286709,1.7,3.5));
#5735=CARTESIAN_POINT('',(2.73448637286709,1.7,3.5));
#5736=CARTESIAN_POINT('Origin',(2.94448637286709,1.7,3.5));
#5737=CARTESIAN_POINT('',(2.73448637286709,1.7,5.));
#5738=CARTESIAN_POINT('',(2.73448637286709,1.7,3.5));
#5739=CARTESIAN_POINT('Origin',(2.94448637286709,1.7,5.));
#5740=CARTESIAN_POINT('Origin',(2.94448637286709,1.7,3.5));
#5741=CARTESIAN_POINT('Origin',(2.0818995585505E-16,3.4,3.5));
#5742=CARTESIAN_POINT('',(-0.21,3.4,3.5));
#5743=CARTESIAN_POINT('Origin',(2.0818995585505E-16,3.4,3.5));
#5744=CARTESIAN_POINT('',(-0.21,3.4,5.));
#5745=CARTESIAN_POINT('',(-0.21,3.4,3.5));
#5746=CARTESIAN_POINT('Origin',(2.0818995585505E-16,3.4,5.));
#5747=CARTESIAN_POINT('Origin',(2.22044604925031E-16,3.4,3.5));
#5748=CARTESIAN_POINT('Origin',(-2.94448637286709,1.7,3.5));
#5749=CARTESIAN_POINT('',(-3.15448637286709,1.7,3.5));
#5750=CARTESIAN_POINT('Origin',(-2.94448637286709,1.7,3.5));
#5751=CARTESIAN_POINT('',(-3.15448637286709,1.7,5.));
#5752=CARTESIAN_POINT('',(-3.15448637286709,1.7,3.5));
#5753=CARTESIAN_POINT('Origin',(-2.94448637286709,1.7,5.));
#5754=CARTESIAN_POINT('Origin',(-2.94448637286709,1.7,3.5));
#5755=CARTESIAN_POINT('Origin',(-2.94448637286709,-1.7,3.5));
#5756=CARTESIAN_POINT('',(-3.15448637286709,-1.7,3.5));
#5757=CARTESIAN_POINT('Origin',(-2.94448637286709,-1.7,3.5));
#5758=CARTESIAN_POINT('',(-3.15448637286709,-1.7,5.));
#5759=CARTESIAN_POINT('',(-3.15448637286709,-1.7,3.5));
#5760=CARTESIAN_POINT('Origin',(-2.94448637286709,-1.7,5.));
#5761=CARTESIAN_POINT('Origin',(-2.94448637286709,-1.7,3.5));
#5762=CARTESIAN_POINT('Origin',(2.94448637286709,-1.7,3.5));
#5763=CARTESIAN_POINT('',(2.73448637286709,-1.7,3.5));
#5764=CARTESIAN_POINT('Origin',(2.94448637286709,-1.7,3.5));
#5765=CARTESIAN_POINT('',(2.73448637286709,-1.7,5.));
#5766=CARTESIAN_POINT('',(2.73448637286709,-1.7,3.5));
#5767=CARTESIAN_POINT('Origin',(2.94448637286709,-1.7,5.));
#5768=CARTESIAN_POINT('Origin',(2.94448637286709,-1.7,3.5));
#5769=CARTESIAN_POINT('Origin',(-0.1,0.,3.9));
#5770=CARTESIAN_POINT('',(2.5,0.,3.5));
#5771=CARTESIAN_POINT('',(2.5,0.,4.3));
#5772=CARTESIAN_POINT('Origin',(2.5,0.,3.9));
#5773=CARTESIAN_POINT('Ctrl Pts',(2.5,2.77555756156289E-17,4.3));
#5774=CARTESIAN_POINT('Ctrl Pts',(2.5,-0.0503173531062473,4.3));
#5775=CARTESIAN_POINT('Ctrl Pts',(2.49832635585429,-0.103929980260481,4.28992638341895));
#5776=CARTESIAN_POINT('Ctrl Pts',(2.49227754123301,-0.202456609487086,4.24907785041389));
#5777=CARTESIAN_POINT('Ctrl Pts',(2.48798680132732,-0.247377744540872,4.21830768040837));
#5778=CARTESIAN_POINT('Ctrl Pts',(2.47991004659989,-0.318308483288254,4.14737694166098));
#5779=CARTESIAN_POINT('Ctrl Pts',(2.47559507764305,-0.3490780234852,4.10245615200085));
#5780=CARTESIAN_POINT('Ctrl Pts',(2.46949065540042,-0.389926098864548,4.00393070664371));
#5781=CARTESIAN_POINT('Ctrl Pts',(2.46779253585061,-0.4,3.95031849222446));
#5782=CARTESIAN_POINT('Ctrl Pts',(2.46779253585061,-0.4,3.84968150777554));
#5783=CARTESIAN_POINT('Ctrl Pts',(2.46949065540042,-0.389926098864548,3.79606929335629));
#5784=CARTESIAN_POINT('Ctrl Pts',(2.47559507764305,-0.3490780234852,3.69754384799915));
#5785=CARTESIAN_POINT('Ctrl Pts',(2.47991004659989,-0.318308483288254,3.65262305833902));
#5786=CARTESIAN_POINT('Ctrl Pts',(2.48798680132732,-0.247377744540872,3.58169231959163));
#5787=CARTESIAN_POINT('Ctrl Pts',(2.49227754123301,-0.202456609487086,3.55092214958611));
#5788=CARTESIAN_POINT('Ctrl Pts',(2.49832635585429,-0.103929980260481,3.51007361658105));
#5789=CARTESIAN_POINT('Ctrl Pts',(2.5,-0.0503173531062475,3.5));
#5790=CARTESIAN_POINT('Ctrl Pts',(2.5,-1.52655665885959E-16,3.5));
#5791=CARTESIAN_POINT('Origin',(-0.1,0.,3.9));
#5792=CARTESIAN_POINT('Origin',(2.5,0.,3.9));
#5793=CARTESIAN_POINT('Ctrl Pts',(2.5,-2.77555756156289E-17,3.5));
#5794=CARTESIAN_POINT('Ctrl Pts',(2.5,0.0503173531062474,3.5));
#5795=CARTESIAN_POINT('Ctrl Pts',(2.49832635585429,0.103929980260481,3.51007361658105));
#5796=CARTESIAN_POINT('Ctrl Pts',(2.49227754123301,0.202456609487086,3.55092214958611));
#5797=CARTESIAN_POINT('Ctrl Pts',(2.48798680132732,0.247377744540872,3.58169231959163));
#5798=CARTESIAN_POINT('Ctrl Pts',(2.47991004659989,0.318308483288254,3.65262305833902));
#5799=CARTESIAN_POINT('Ctrl Pts',(2.47559507764305,0.3490780234852,3.69754384799915));
#5800=CARTESIAN_POINT('Ctrl Pts',(2.46949065540042,0.389926098864548,3.79606929335629));
#5801=CARTESIAN_POINT('Ctrl Pts',(2.46779253585061,0.4,3.84968150777554));
#5802=CARTESIAN_POINT('Ctrl Pts',(2.46779253585061,0.4,3.9));
#5803=CARTESIAN_POINT('Ctrl Pts',(2.46779253585061,0.4,3.95031849222446));
#5804=CARTESIAN_POINT('Ctrl Pts',(2.46949065540042,0.389926098864548,4.00393070664371));
#5805=CARTESIAN_POINT('Ctrl Pts',(2.47559507764305,0.3490780234852,4.10245615200085));
#5806=CARTESIAN_POINT('Ctrl Pts',(2.47991004659989,0.318308483288254,4.14737694166098));
#5807=CARTESIAN_POINT('Ctrl Pts',(2.48798680132732,0.247377744540872,4.21830768040837));
#5808=CARTESIAN_POINT('Ctrl Pts',(2.49227754123301,0.202456609487086,4.24907785041389));
#5809=CARTESIAN_POINT('Ctrl Pts',(2.49832635585429,0.103929980260481,4.28992638341895));
#5810=CARTESIAN_POINT('Ctrl Pts',(2.5,0.0503173531062475,4.3));
#5811=CARTESIAN_POINT('Ctrl Pts',(2.5,8.32667268468867E-17,4.3));
#5812=CARTESIAN_POINT('Origin',(2.5,0.,3.9));
#5813=CARTESIAN_POINT('',(2.5,-8.38883057415937E-17,4.585));
#5814=CARTESIAN_POINT('',(2.5,0.,3.2));
#5815=CARTESIAN_POINT('',(2.5,0.,3.215));
#5816=CARTESIAN_POINT('Origin',(2.5,0.,3.9));
#5817=CARTESIAN_POINT('',(2.5,0.,3.2));
#5818=CARTESIAN_POINT('Origin',(2.5,0.,3.9));
#5819=CARTESIAN_POINT('',(2.5,0.,3.2));
#5820=CARTESIAN_POINT('Origin',(2.5,0.,3.9));
#5821=CARTESIAN_POINT('',(2.5,0.,3.2));
#5822=CARTESIAN_POINT('Origin',(2.5,0.,3.9));
#5823=CARTESIAN_POINT('',(4.,-8.38883057415937E-17,4.585));
#5824=CARTESIAN_POINT('',(2.5,-8.38883057415937E-17,4.585));
#5825=CARTESIAN_POINT('',(3.94091042780726,0.685,3.9));
#5826=CARTESIAN_POINT('Ctrl Pts',(3.94091042780726,0.685,3.9));
#5827=CARTESIAN_POINT('Ctrl Pts',(3.94091042780726,0.685,3.81380574680012));
#5828=CARTESIAN_POINT('Ctrl Pts',(3.94403084813346,0.667739203937252,3.7219849815769));
#5829=CARTESIAN_POINT('Ctrl Pts',(3.95523876756334,0.597780269847898,3.55326702036063));
#5830=CARTESIAN_POINT('Ctrl Pts',(3.96315754832666,0.545091192335771,3.4763549021102));
#5831=CARTESIAN_POINT('Ctrl Pts',(3.97797250301845,0.423646908301837,3.35491061807627));
#5832=CARTESIAN_POINT('Ctrl Pts',(3.98584030517825,0.346734013912698,3.30222012067742));
#5833=CARTESIAN_POINT('Ctrl Pts',(3.99693115404432,0.178013382290042,3.2322601559763));
#5834=CARTESIAN_POINT('Ctrl Pts',(4.,0.086191683382974,3.215));
#5835=CARTESIAN_POINT('Ctrl Pts',(4.,-0.086191683382974,3.215));
#5836=CARTESIAN_POINT('Ctrl Pts',(3.99693115404432,-0.178013382290042,3.2322601559763));
#5837=CARTESIAN_POINT('Ctrl Pts',(3.98584030517825,-0.346734013912697,3.30222012067742));
#5838=CARTESIAN_POINT('Ctrl Pts',(3.97797250301845,-0.423646908301837,3.35491061807627));
#5839=CARTESIAN_POINT('Ctrl Pts',(3.96315754832666,-0.545091192335771,3.4763549021102));
#5840=CARTESIAN_POINT('Ctrl Pts',(3.95523876756334,-0.597780269847898,3.55326702036063));
#5841=CARTESIAN_POINT('Ctrl Pts',(3.94403084813346,-0.667739203937252,3.7219849815769));
#5842=CARTESIAN_POINT('Ctrl Pts',(3.94091042780726,-0.685,3.81380574680012));
#5843=CARTESIAN_POINT('Ctrl Pts',(3.94091042780726,-0.685,3.98619425319988));
#5844=CARTESIAN_POINT('Ctrl Pts',(3.94403084813346,-0.667739203937252,4.0780150184231));
#5845=CARTESIAN_POINT('Ctrl Pts',(3.95523876756334,-0.597780269847898,4.24673297963937));
#5846=CARTESIAN_POINT('Ctrl Pts',(3.96315754832666,-0.545091192335771,4.3236450978898));
#5847=CARTESIAN_POINT('Ctrl Pts',(3.97797250301844,-0.423646908301837,4.44508938192373));
#5848=CARTESIAN_POINT('Ctrl Pts',(3.98584030517825,-0.346734013912698,4.49777987932258));
#5849=CARTESIAN_POINT('Ctrl Pts',(3.99693115404432,-0.178013382290042,4.5677398440237));
#5850=CARTESIAN_POINT('Ctrl Pts',(4.,-0.0861916833829741,4.585));
#5851=CARTESIAN_POINT('Ctrl Pts',(4.,0.,4.585));
#5852=CARTESIAN_POINT('Ctrl Pts',(4.,-1.94289029309402E-16,4.585));
#5853=CARTESIAN_POINT('Ctrl Pts',(4.,0.0861916833829739,4.585));
#5854=CARTESIAN_POINT('Ctrl Pts',(3.99693115404432,0.178013382290042,4.5677398440237));
#5855=CARTESIAN_POINT('Ctrl Pts',(3.98584030517825,0.346734013912697,4.49777987932258));
#5856=CARTESIAN_POINT('Ctrl Pts',(3.97797250301844,0.423646908301837,4.44508938192373));
#5857=CARTESIAN_POINT('Ctrl Pts',(3.96315754832666,0.545091192335771,4.3236450978898));
#5858=CARTESIAN_POINT('Ctrl Pts',(3.95523876756334,0.597780269847898,4.24673297963937));
#5859=CARTESIAN_POINT('Ctrl Pts',(3.94403084813346,0.667739203937252,4.0780150184231));
#5860=CARTESIAN_POINT('Ctrl Pts',(3.94091042780726,0.685,3.98619425319988));
#5861=CARTESIAN_POINT('Ctrl Pts',(3.94091042780726,0.685,3.9));
#5862=CARTESIAN_POINT('Origin',(-2.6,0.,1.9));
#5863=CARTESIAN_POINT('',(-2.5,-4.89858719658941E-17,2.3));
#5864=CARTESIAN_POINT('Origin',(-2.5,0.,1.9));
#5865=CARTESIAN_POINT('',(-0.8,-5.91874055024832E-17,2.3));
#5866=CARTESIAN_POINT('',(-2.6,-4.89858719658941E-17,2.3));
#5867=CARTESIAN_POINT('',(-0.8,9.79717439317883E-17,1.5));
#5868=CARTESIAN_POINT('Ctrl Pts',(-0.8,-1.38777878078145E-17,1.5));
#5869=CARTESIAN_POINT('Ctrl Pts',(-0.8,-0.0511821204434756,1.5));
#5870=CARTESIAN_POINT('Ctrl Pts',(-0.794636787340262,-0.105178030195542,
1.51041443765235));
#5871=CARTESIAN_POINT('Ctrl Pts',(-0.775305936415791,-0.20349630324575,
1.55153396803017));
#5872=CARTESIAN_POINT('Ctrl Pts',(-0.761546644028199,-0.247878667922505,
1.58219324297327));
#5873=CARTESIAN_POINT('Ctrl Pts',(-0.735080187019535,-0.317902331252414,
1.65221690630318));
#5874=CARTESIAN_POINT('Ctrl Pts',(-0.720478404984272,-0.34849148389449,
1.69656705619687));
#5875=CARTESIAN_POINT('Ctrl Pts',(-0.699130174381174,-0.389554233790704,
1.79474455949469));
#5876=CARTESIAN_POINT('Ctrl Pts',(-0.692820323027551,-0.4,1.8486779732158));
#5877=CARTESIAN_POINT('Ctrl Pts',(-0.692820323027551,-0.4,1.9513220267842));
#5878=CARTESIAN_POINT('Ctrl Pts',(-0.699130174381174,-0.389554233790704,
2.00525544050531));
#5879=CARTESIAN_POINT('Ctrl Pts',(-0.720478404984272,-0.348491483894491,
2.10343294380313));
#5880=CARTESIAN_POINT('Ctrl Pts',(-0.735080187019535,-0.317902331252414,
2.14778309369682));
#5881=CARTESIAN_POINT('Ctrl Pts',(-0.761546644028199,-0.247878667922505,
2.21780675702673));
#5882=CARTESIAN_POINT('Ctrl Pts',(-0.775305936415791,-0.20349630324575,
2.24846603196983));
#5883=CARTESIAN_POINT('Ctrl Pts',(-0.794636787340262,-0.105178030195542,
2.28958556234765));
#5884=CARTESIAN_POINT('Ctrl Pts',(-0.8,-0.0511821204434756,2.3));
#5885=CARTESIAN_POINT('Ctrl Pts',(-0.8,-6.93889390390723E-17,2.3));
#5886=CARTESIAN_POINT('',(-0.925,-1.1327982892113E-16,1.5));
#5887=CARTESIAN_POINT('',(-2.6,0.,1.5));
#5888=CARTESIAN_POINT('',(-2.6,0.,1.5));
#5889=CARTESIAN_POINT('Ctrl Pts',(-0.8,-8.32667268468867E-17,2.3));
#5890=CARTESIAN_POINT('Ctrl Pts',(-0.8,0.0511821204434754,2.3));
#5891=CARTESIAN_POINT('Ctrl Pts',(-0.794636787340262,0.105178030195542,
2.28958556234765));
#5892=CARTESIAN_POINT('Ctrl Pts',(-0.775305936415791,0.20349630324575,2.24846603196983));
#5893=CARTESIAN_POINT('Ctrl Pts',(-0.761546644028199,0.247878667922505,
2.21780675702673));
#5894=CARTESIAN_POINT('Ctrl Pts',(-0.735080187019535,0.317902331252414,
2.14778309369682));
#5895=CARTESIAN_POINT('Ctrl Pts',(-0.720478404984272,0.348491483894491,
2.10343294380313));
#5896=CARTESIAN_POINT('Ctrl Pts',(-0.699130174381174,0.389554233790704,
2.00525544050531));
#5897=CARTESIAN_POINT('Ctrl Pts',(-0.692820323027551,0.4,1.9513220267842));
#5898=CARTESIAN_POINT('Ctrl Pts',(-0.692820323027551,0.4,1.9));
#5899=CARTESIAN_POINT('Ctrl Pts',(-0.692820323027551,0.4,1.8486779732158));
#5900=CARTESIAN_POINT('Ctrl Pts',(-0.699130174381174,0.389554233790704,
1.79474455949469));
#5901=CARTESIAN_POINT('Ctrl Pts',(-0.720478404984272,0.34849148389449,1.69656705619687));
#5902=CARTESIAN_POINT('Ctrl Pts',(-0.735080187019535,0.317902331252414,
1.65221690630318));
#5903=CARTESIAN_POINT('Ctrl Pts',(-0.761546644028199,0.247878667922505,
1.58219324297327));
#5904=CARTESIAN_POINT('Ctrl Pts',(-0.775305936415792,0.20349630324575,1.55153396803017));
#5905=CARTESIAN_POINT('Ctrl Pts',(-0.794636787340262,0.105178030195542,
1.51041443765235));
#5906=CARTESIAN_POINT('Ctrl Pts',(-0.8,0.0511821204434755,1.5));
#5907=CARTESIAN_POINT('Ctrl Pts',(-0.8,-5.55111512312578E-17,1.5));
#5908=CARTESIAN_POINT('Origin',(0.,0.,1.4));
#5909=CARTESIAN_POINT('Origin',(0.,0.,1.5));
#5910=CARTESIAN_POINT('',(-0.8,-9.79717439317883E-17,2.4));
#5911=CARTESIAN_POINT('',(-0.8,-9.79717439317883E-17,1.4));
#5912=CARTESIAN_POINT('Origin',(0.,0.,2.4));
#5913=CARTESIAN_POINT('Origin',(-4.1,0.,1.9));
#5914=CARTESIAN_POINT('',(-3.94091042780726,0.685,1.9));
#5915=CARTESIAN_POINT('',(-4.,-8.38883057415937E-17,2.585));
#5916=CARTESIAN_POINT('Ctrl Pts',(-3.94091042780726,0.685,1.9));
#5917=CARTESIAN_POINT('Ctrl Pts',(-3.94091042780726,0.685,1.98619425319988));
#5918=CARTESIAN_POINT('Ctrl Pts',(-3.94403084813346,0.667739203937252,2.07801501842309));
#5919=CARTESIAN_POINT('Ctrl Pts',(-3.95523876756334,0.597780269847899,2.24673297963937));
#5920=CARTESIAN_POINT('Ctrl Pts',(-3.96315754832666,0.545091192335771,2.3236450978898));
#5921=CARTESIAN_POINT('Ctrl Pts',(-3.97797250301844,0.423646908301837,2.44508938192373));
#5922=CARTESIAN_POINT('Ctrl Pts',(-3.98584030517825,0.346734013912698,2.49777987932258));
#5923=CARTESIAN_POINT('Ctrl Pts',(-3.99693115404432,0.178013382290042,2.5677398440237));
#5924=CARTESIAN_POINT('Ctrl Pts',(-4.,0.0861916833829741,2.585));
#5925=CARTESIAN_POINT('Ctrl Pts',(-4.,2.77555756156289E-17,2.585));
#5926=CARTESIAN_POINT('',(-4.,-3.14318298868543E-16,1.215));
#5927=CARTESIAN_POINT('Ctrl Pts',(-4.,-1.38777878078145E-16,1.215));
#5928=CARTESIAN_POINT('Ctrl Pts',(-4.,0.0861916833829738,1.215));
#5929=CARTESIAN_POINT('Ctrl Pts',(-3.99693115404432,0.178013382290042,1.2322601559763));
#5930=CARTESIAN_POINT('Ctrl Pts',(-3.98584030517825,0.346734013912697,1.30222012067742));
#5931=CARTESIAN_POINT('Ctrl Pts',(-3.97797250301844,0.423646908301837,1.35491061807627));
#5932=CARTESIAN_POINT('Ctrl Pts',(-3.96315754832666,0.545091192335771,1.4763549021102));
#5933=CARTESIAN_POINT('Ctrl Pts',(-3.95523876756334,0.597780269847898,1.55326702036063));
#5934=CARTESIAN_POINT('Ctrl Pts',(-3.94403084813346,0.667739203937252,1.7219849815769));
#5935=CARTESIAN_POINT('Ctrl Pts',(-3.94091042780726,0.685,1.81380574680012));
#5936=CARTESIAN_POINT('Ctrl Pts',(-3.94091042780726,0.685,1.9));
#5937=CARTESIAN_POINT('Ctrl Pts',(-4.,1.11022302462516E-16,2.585));
#5938=CARTESIAN_POINT('Ctrl Pts',(-4.,-0.0861916833829739,2.585));
#5939=CARTESIAN_POINT('Ctrl Pts',(-3.99693115404432,-0.178013382290042,
2.5677398440237));
#5940=CARTESIAN_POINT('Ctrl Pts',(-3.98584030517825,-0.346734013912697,
2.49777987932258));
#5941=CARTESIAN_POINT('Ctrl Pts',(-3.97797250301844,-0.423646908301837,
2.44508938192373));
#5942=CARTESIAN_POINT('Ctrl Pts',(-3.96315754832666,-0.545091192335771,
2.3236450978898));
#5943=CARTESIAN_POINT('Ctrl Pts',(-3.95523876756334,-0.597780269847899,
2.24673297963937));
#5944=CARTESIAN_POINT('Ctrl Pts',(-3.94403084813346,-0.667739203937252,
2.07801501842309));
#5945=CARTESIAN_POINT('Ctrl Pts',(-3.94091042780726,-0.685,1.98619425319988));
#5946=CARTESIAN_POINT('Ctrl Pts',(-3.94091042780726,-0.685,1.81380574680012));
#5947=CARTESIAN_POINT('Ctrl Pts',(-3.94403084813346,-0.667739203937252,
1.7219849815769));
#5948=CARTESIAN_POINT('Ctrl Pts',(-3.95523876756334,-0.597780269847898,
1.55326702036063));
#5949=CARTESIAN_POINT('Ctrl Pts',(-3.96315754832666,-0.545091192335771,
1.4763549021102));
#5950=CARTESIAN_POINT('Ctrl Pts',(-3.97797250301844,-0.423646908301837,
1.35491061807627));
#5951=CARTESIAN_POINT('Ctrl Pts',(-3.98584030517825,-0.346734013912697,
1.30222012067742));
#5952=CARTESIAN_POINT('Ctrl Pts',(-3.99693115404432,-0.178013382290042,
1.2322601559763));
#5953=CARTESIAN_POINT('Ctrl Pts',(-4.,-0.0861916833829742,1.215));
#5954=CARTESIAN_POINT('Ctrl Pts',(-4.,-2.22044604925031E-16,1.215));
#5955=CARTESIAN_POINT('',(-2.5,-8.38883057415937E-17,2.585));
#5956=CARTESIAN_POINT('',(-4.1,-8.38883057415937E-17,2.585));
#5957=CARTESIAN_POINT('Origin',(-2.5,0.,1.9));
#5958=CARTESIAN_POINT('Origin',(-2.5,0.,1.9));
#5959=CARTESIAN_POINT('Origin',(0.,-3.,0.9));
#5960=CARTESIAN_POINT('',(-0.165,-3.,1.));
#5961=CARTESIAN_POINT('Origin',(0.,-3.,1.));
#5962=CARTESIAN_POINT('',(-0.165,-3.,2.1));
#5963=CARTESIAN_POINT('',(-0.165,-3.,0.9));
#5964=CARTESIAN_POINT('Origin',(0.,-3.,2.1));
#5965=CARTESIAN_POINT('Origin',(0.,-3.,2.1));
#5966=CARTESIAN_POINT('Origin',(0.,3.,0.9));
#5967=CARTESIAN_POINT('',(-0.165,3.,1.));
#5968=CARTESIAN_POINT('Origin',(0.,3.,1.));
#5969=CARTESIAN_POINT('',(-0.165,3.,2.1));
#5970=CARTESIAN_POINT('',(-0.165,3.,0.9));
#5971=CARTESIAN_POINT('Origin',(0.,3.,2.1));
#5972=CARTESIAN_POINT('Origin',(0.,3.,2.1));
#5973=CARTESIAN_POINT('Origin',(0.,0.,0.9));
#5974=CARTESIAN_POINT('',(-0.925,-1.1327982892113E-16,1.));
#5975=CARTESIAN_POINT('Origin',(0.,0.,1.));
#5976=CARTESIAN_POINT('',(-0.925,-1.1327982892113E-16,0.9));
#5977=CARTESIAN_POINT('Origin',(0.,0.,1.5));
#5978=CARTESIAN_POINT('Origin',(0.,0.,1.5));
#5979=CARTESIAN_POINT('Origin',(0.,0.,2.3));
#5980=CARTESIAN_POINT('',(-0.6,-7.34788079488412E-17,2.4));
#5981=CARTESIAN_POINT('Origin',(0.,0.,2.4));
#5982=CARTESIAN_POINT('',(-0.6,7.34788079488412E-17,3.2));
#5983=CARTESIAN_POINT('',(-0.6,-7.34788079488412E-17,2.3));
#5984=CARTESIAN_POINT('Origin',(0.,0.,3.2));
#5985=CARTESIAN_POINT('Origin',(0.,0.,2.4));
#5986=CARTESIAN_POINT('Origin',(0.,0.,3.2));
#5987=CARTESIAN_POINT('',(2.5,0.,3.2));
#5988=CARTESIAN_POINT('Origin',(0.,0.,3.2));
#5989=CARTESIAN_POINT('',(2.5,0.,3.2));
#5990=CARTESIAN_POINT('',(2.5,0.,5.));
#5991=CARTESIAN_POINT('',(2.5,0.,3.2));
#5992=CARTESIAN_POINT('Origin',(0.,0.,5.));
#5993=CARTESIAN_POINT('Origin',(0.,0.,3.2));
#5994=CARTESIAN_POINT('Origin',(0.,0.,1.));
#5995=CARTESIAN_POINT('',(-4.,-4.89858719658941E-16,5.));
#5996=CARTESIAN_POINT('Origin',(0.,0.,5.));
#5997=CARTESIAN_POINT('',(-4.,-4.89858719658941E-16,1.));
#5998=CARTESIAN_POINT('',(-4.,-4.89858719658941E-16,1.));
#5999=CARTESIAN_POINT('',(-4.,-4.89858719658941E-16,1.));
#6000=CARTESIAN_POINT('Origin',(0.,0.,1.));
#6001=CARTESIAN_POINT('Origin',(0.,0.,5.));
#6002=CARTESIAN_POINT('Origin',(0.,0.,1.));
#6003=CARTESIAN_POINT('',(0.,0.,0.));
#6004=CARTESIAN_POINT('Origin',(0.,0.,1.));
#6005=CARTESIAN_POINT('',(-1.3,-1.59204083889156E-16,1.));
#6006=CARTESIAN_POINT('Origin',(0.,0.,1.));
#6007=CARTESIAN_POINT('',(-1.,-1.22464679914735E-16,1.));
#6008=CARTESIAN_POINT('Origin',(0.,0.,1.));
#6009=CARTESIAN_POINT('Origin',(0.,0.,0.8));
#6010=CARTESIAN_POINT('',(-1.3,-1.59204083889156E-16,0.8));
#6011=CARTESIAN_POINT('',(-1.3,-1.59204083889156E-16,0.8));
#6012=CARTESIAN_POINT('Origin',(0.,0.,0.8));
#6013=CARTESIAN_POINT('Origin',(0.,0.,0.8));
#6014=CARTESIAN_POINT('Origin',(0.,0.,1.));
#6015=CARTESIAN_POINT('',(-1.,-1.22464679914735E-16,1.4));
#6016=CARTESIAN_POINT('Origin',(0.,0.,1.4));
#6017=CARTESIAN_POINT('',(-1.,-1.22464679914735E-16,1.));
#6018=CARTESIAN_POINT('Origin',(0.,0.,1.4));
#6019=CARTESIAN_POINT('',(0.,0.,0.));
#6020=CARTESIAN_POINT('Origin',(0.,0.,2.4));
#6021=CARTESIAN_POINT('',(-0.2,-2.44929359829471E-17,3.2));
#6022=CARTESIAN_POINT('Origin',(0.,0.,3.2));
#6023=CARTESIAN_POINT('',(-0.2,-2.44929359829471E-17,2.4));
#6024=CARTESIAN_POINT('',(-0.2,-2.44929359829471E-17,2.4));
#6025=CARTESIAN_POINT('Origin',(0.,0.,2.4));
#6026=CARTESIAN_POINT('Origin',(0.,0.,2.4));
#6027=CARTESIAN_POINT('',(-0.6,-7.34788079488412E-17,3.2));
#6028=CARTESIAN_POINT('Origin',(0.,0.,3.2));
#6029=CARTESIAN_POINT('',(-0.6,-7.34788079488412E-17,2.4));
#6030=CARTESIAN_POINT('',(-0.6,-7.34788079488412E-17,2.4));
#6031=CARTESIAN_POINT('Origin',(0.,0.,2.4));
#6032=CARTESIAN_POINT('Origin',(0.,0.,3.2));
#6033=CARTESIAN_POINT('Origin',(0.,0.,2.4));
#6034=CARTESIAN_POINT('',(0.,0.,0.));
#6035=CARTESIAN_POINT('Origin',(0.,0.,5.3));
#6036=CARTESIAN_POINT('',(-0.4,-4.89858719658941E-17,5.3));
#6037=CARTESIAN_POINT('Origin',(0.,0.,5.3));
#6038=CARTESIAN_POINT('',(-0.15,1.83697019872103E-17,5.3));
#6039=CARTESIAN_POINT('Origin',(0.,0.,5.3));
#6040=CARTESIAN_POINT('Origin',(0.,0.,5.3));
#6041=CARTESIAN_POINT('',(-0.4,-4.89858719658941E-17,5.5));
#6042=CARTESIAN_POINT('Origin',(0.,0.,5.5));
#6043=CARTESIAN_POINT('',(-0.4,-4.89858719658941E-17,5.3));
#6044=CARTESIAN_POINT('Origin',(0.,0.,4.8));
#6045=CARTESIAN_POINT('',(-0.4,-4.89858719658941E-17,4.8));
#6046=CARTESIAN_POINT('Origin',(0.,0.,4.8));
#6047=CARTESIAN_POINT('',(-0.15,-1.83697019872103E-17,4.8));
#6048=CARTESIAN_POINT('Origin',(0.,0.,4.8));
#6049=CARTESIAN_POINT('Origin',(0.,0.,4.6));
#6050=CARTESIAN_POINT('',(-0.4,-4.89858719658941E-17,4.6));
#6051=CARTESIAN_POINT('Origin',(0.,0.,4.6));
#6052=CARTESIAN_POINT('',(-0.15,1.83697019872103E-17,4.6));
#6053=CARTESIAN_POINT('Origin',(0.,0.,4.6));
#6054=CARTESIAN_POINT('Origin',(0.,0.,4.6));
#6055=CARTESIAN_POINT('',(-0.4,-4.89858719658941E-17,4.6));
#6056=CARTESIAN_POINT('Origin',(0.,0.,2.4));
#6057=CARTESIAN_POINT('',(-0.15,-1.83697019872103E-17,2.4));
#6058=CARTESIAN_POINT('',(-0.15,-1.83697019872103E-17,2.4));
#6059=CARTESIAN_POINT('Origin',(0.,0.,2.4));
#6060=CARTESIAN_POINT('Origin',(0.,0.,2.4));
#6061=CARTESIAN_POINT('',(-0.15,-1.83697019872103E-17,2.4));
#6062=CARTESIAN_POINT('Origin',(0.,0.,5.5));
#6063=CARTESIAN_POINT('Origin',(0.,0.,2.2));
#6064=CARTESIAN_POINT('',(-0.4,-4.89858719658941E-17,2.4));
#6065=CARTESIAN_POINT('Origin',(0.,0.,2.4));
#6066=CARTESIAN_POINT('',(-0.4,-4.89858719658941E-17,2.2));
#6067=CARTESIAN_POINT('',(-0.4,-4.89858719658941E-17,2.2));
#6068=CARTESIAN_POINT('Origin',(0.,0.,2.2));
#6069=CARTESIAN_POINT('Origin',(0.,0.,2.4));
#6070=CARTESIAN_POINT('Origin',(0.,0.,2.2));
#6071=CARTESIAN_POINT('',(0.,0.,0.));
#6072=CARTESIAN_POINT('Ctrl Pts',(0.299999683646987,0.00234130352927725,
1.40009150124657));
#6073=CARTESIAN_POINT('Ctrl Pts',(0.299992075807792,0.058646317336039,1.40449918252257));
#6074=CARTESIAN_POINT('Ctrl Pts',(0.267703823976176,0.170873854805974,1.41332597689034));
#6075=CARTESIAN_POINT('Ctrl Pts',(0.136388292868123,0.288427001435921,1.42662720914847));
#6076=CARTESIAN_POINT('Ctrl Pts',(-0.0380600582278086,0.318117946543192,
1.43998475699785));
#6077=CARTESIAN_POINT('Ctrl Pts',(-0.202303265104397,0.250195717548651,
1.45340015631867));
#6078=CARTESIAN_POINT('Ctrl Pts',(-0.305668184856449,0.104682534491432,
1.46687214536364));
#6079=CARTESIAN_POINT('Ctrl Pts',(-0.315820032591246,-0.0743007733969036,
1.48040059247731));
#6080=CARTESIAN_POINT('Ctrl Pts',(-0.250581817185145,-0.192431453073831,
1.49058865012208));
#6081=CARTESIAN_POINT('Ctrl Pts',(-0.184885616277594,-0.249388366415835,
1.49739790674125));
#6082=CARTESIAN_POINT('Ctrl Pts',(-0.148390241821198,-0.273082371347815,
1.50080595723938));
#6083=CARTESIAN_POINT('Ctrl Pts',(-0.108871032283292,-0.29139234917315,
1.50421741983629));
#6084=CARTESIAN_POINT('Ctrl Pts',(-0.0069453324122751,-0.322535646049005,
1.51256485573429));
#6085=CARTESIAN_POINT('Ctrl Pts',(0.173036139719135,-0.295879163364944,
1.52588654224678));
#6086=CARTESIAN_POINT('Ctrl Pts',(0.329381275573112,-0.0995231210697565,
1.54425036939462));
#6087=CARTESIAN_POINT('Ctrl Pts',(0.312519823715869,0.130664619012925,1.56116776183919));
#6088=CARTESIAN_POINT('Ctrl Pts',(0.175623409891217,0.283196568811908,1.57661184582646));
#6089=CARTESIAN_POINT('Ctrl Pts',(-0.00170640174969724,0.334465005486407,
1.59056005485894));
#6090=CARTESIAN_POINT('Ctrl Pts',(-0.180023541764348,0.283195393823563,
1.60455538622492));
#6091=CARTESIAN_POINT('Ctrl Pts',(-0.304003293840334,0.144546913461868,
1.61859632997908));
#6092=CARTESIAN_POINT('Ctrl Pts',(-0.335368767729676,-0.0394152680933303,
1.63268129545808));
#6093=CARTESIAN_POINT('Ctrl Pts',(-0.263809464751215,-0.212364713608931,
1.64680860320332));
#6094=CARTESIAN_POINT('Ctrl Pts',(-0.110777353802162,-0.321042679653587,
1.66097649136357));
#6095=CARTESIAN_POINT('Ctrl Pts',(0.0771377319574853,-0.331662145388596,
1.67518312328143));
#6096=CARTESIAN_POINT('Ctrl Pts',(0.242310499059917,-0.240422185372272,
1.68942658430208));
#6097=CARTESIAN_POINT('Ctrl Pts',(0.333965165875749,-0.0749639048060816,
1.70370489167579));
#6098=CARTESIAN_POINT('Ctrl Pts',(0.323334808639096,0.114391665751362,1.71801599173701));
#6099=CARTESIAN_POINT('Ctrl Pts',(0.213428807823085,0.269386973572793,1.73235777220482));
#6100=CARTESIAN_POINT('Ctrl Pts',(0.0375551957208218,0.342290293088701,
1.74672805867088));
#6101=CARTESIAN_POINT('Ctrl Pts',(-0.150552157108958,0.310435266995363,
1.76112462104241));
#6102=CARTESIAN_POINT('Ctrl Pts',(-0.292943546037226,0.183080826664645,
1.7755451807512));
#6103=CARTESIAN_POINT('Ctrl Pts',(-0.345971724616545,-0.000755050169826696,
1.78998741229651));
#6104=CARTESIAN_POINT('Ctrl Pts',(-0.292969625414991,-0.184869584225357,
1.80444894933381));
#6105=CARTESIAN_POINT('Ctrl Pts',(-0.149964130695888,-0.312702949838195,
1.81892738366057));
#6106=CARTESIAN_POINT('Ctrl Pts',(0.0393278383702601,-0.344893411306051,
1.83342028161105));
#6107=CARTESIAN_POINT('Ctrl Pts',(0.216880569645654,-0.271353329755712,
1.84792517694669));
#6108=CARTESIAN_POINT('Ctrl Pts',(0.32816306590606,-0.114557947655581,1.86243958044385));
#6109=CARTESIAN_POINT('Ctrl Pts',(0.338976565498085,0.077604733921516,1.87696098559129));
#6110=CARTESIAN_POINT('Ctrl Pts',(0.245857394029791,0.245901091257368,1.8914868739057));
#6111=CARTESIAN_POINT('Ctrl Pts',(0.0587650041824393,0.349754038023421,
1.90762891978624));
#6112=CARTESIAN_POINT('Ctrl Pts',(-0.181113967151586,0.314103429348402,
1.92538434383923));
#6113=CARTESIAN_POINT('Ctrl Pts',(-0.3457209249242,0.106820407791971,1.94474686926749));
#6114=CARTESIAN_POINT('Ctrl Pts',(-0.329429326627219,-0.112545408830404,
1.96087146849268));
#6115=CARTESIAN_POINT('Ctrl Pts',(-0.229624239431613,-0.246663510889421,
1.97376168226292));
#6116=CARTESIAN_POINT('Ctrl Pts',(-0.0883709022792632,-0.335964900532689,
1.98664460529397));
#6117=CARTESIAN_POINT('Ctrl Pts',(0.0650538569064664,-0.336061455964098,
1.99790631348129));
#6118=CARTESIAN_POINT('Ctrl Pts',(0.175154846512334,-0.280150232411291,
2.00754964965835));
#6119=CARTESIAN_POINT('Ctrl Pts',(0.240313024233827,-0.230169139256515,
2.01397587403001));
#6120=CARTESIAN_POINT('Ctrl Pts',(0.327278516892606,-0.113059531596934,
2.02521445394406));
#6121=CARTESIAN_POINT('Ctrl Pts',(0.344164783870684,0.104896799870906,2.04124691031968));
#6122=CARTESIAN_POINT('Ctrl Pts',(0.180057434020278,0.310325992459091,2.06044404323233));
#6123=CARTESIAN_POINT('Ctrl Pts',(-0.0568089689745267,0.345505318367412,
2.07799813231589));
#6124=CARTESIAN_POINT('Ctrl Pts',(-0.24141865243425,0.243028671458529,2.09391813720595));
#6125=CARTESIAN_POINT('Ctrl Pts',(-0.332978054716675,0.0773726024996246,
2.1082144881335));
#6126=CARTESIAN_POINT('Ctrl Pts',(-0.322327341410981,-0.111361257795146,
2.12247707319913));
#6127=CARTESIAN_POINT('Ctrl Pts',(-0.213201521733808,-0.265029708724835,
2.13670391728446));
#6128=CARTESIAN_POINT('Ctrl Pts',(-0.0395013579051905,-0.33691517309109,
2.15089294308459));
#6129=CARTESIAN_POINT('Ctrl Pts',(0.145288666887708,-0.305489063077451,
2.16504251556762));
#6130=CARTESIAN_POINT('Ctrl Pts',(0.284599775362727,-0.18083938172608,2.17915024381374));
#6131=CARTESIAN_POINT('Ctrl Pts',(0.318914082780001,-0.0616119635988021,
2.18852795857496));
#6132=CARTESIAN_POINT('Ctrl Pts',(0.318922161847072,-0.0018193816533177,
2.19320865445115));
#6133=CARTESIAN_POINT('Ctrl Pts',(0.293267699450747,0.00234039391484394,
1.40009150124657));
#6134=CARTESIAN_POINT('Ctrl Pts',(0.293260260783866,0.0573933768638441,
1.404401170772));
#6135=CARTESIAN_POINT('Ctrl Pts',(0.261685961222457,0.167106937147775,1.41303112442804));
#6136=CARTESIAN_POINT('Ctrl Pts',(0.133284398422381,0.282057446849938,1.42603808763138));
#6137=CARTESIAN_POINT('Ctrl Pts',(-0.0373291122578389,0.311099769178308,
1.43910259661189));
#6138=CARTESIAN_POINT('Ctrl Pts',(-0.198000217206654,0.244664129919692,
1.45222664056713));
#6139=CARTESIAN_POINT('Ctrl Pts',(-0.299150297118565,0.10228514235472,1.46540970339088));
#6140=CARTESIAN_POINT('Ctrl Pts',(-0.309098158415524,-0.072901218291685,
1.47865182929301));
#6141=CARTESIAN_POINT('Ctrl Pts',(-0.245229011903188,-0.188573983871875,
1.48862820905086));
#6142=CARTESIAN_POINT('Ctrl Pts',(-0.180890303179359,-0.244355141625382,
1.49529690715063));
#6143=CARTESIAN_POINT('Ctrl Pts',(-0.145145442776525,-0.267562223220666,
1.49863493300563));
#6144=CARTESIAN_POINT('Ctrl Pts',(-0.106434830287264,-0.285497864023997,
1.50197663435114));
#6145=CARTESIAN_POINT('Ctrl Pts',(-0.00658463218961376,-0.31600740949559,
1.51015421506047));
#6146=CARTESIAN_POINT('Ctrl Pts',(0.169803335212638,-0.289904551356884,
1.52321054336867));
#6147=CARTESIAN_POINT('Ctrl Pts',(0.323140342136514,-0.0973784285380068,
1.54121822441294));
#6148=CARTESIAN_POINT('Ctrl Pts',(0.306625599321007,0.128498402162331,1.55781889560626));
#6149=CARTESIAN_POINT('Ctrl Pts',(0.172221287437576,0.278283700657156,1.57298361049915));
#6150=CARTESIAN_POINT('Ctrl Pts',(-0.00199515167689712,0.328668835140418,
1.58668730446444));
#6151=CARTESIAN_POINT('Ctrl Pts',(-0.177297430280052,0.278285030800204,
1.60044562410953));
#6152=CARTESIAN_POINT('Ctrl Pts',(-0.299269202723749,0.141909876792653,
1.61425746251936));
#6153=CARTESIAN_POINT('Ctrl Pts',(-0.330162486971795,-0.0391685498718976,
1.62812169321704));
#6154=CARTESIAN_POINT('Ctrl Pts',(-0.259693749447613,-0.209534410414459,
1.64203704930538));
#6155=CARTESIAN_POINT('Ctrl Pts',(-0.108859663184327,-0.316676626843527,
1.65600218178666));
#6156=CARTESIAN_POINT('Ctrl Pts',(0.076505205414545,-0.327173117244501,
1.6700156352621));
#6157=CARTESIAN_POINT('Ctrl Pts',(0.239569384718494,-0.237122125019053,
1.68407584770812));
#6158=CARTESIAN_POINT('Ctrl Pts',(0.330138826176287,-0.0736687244436319,
1.69818173535813));
#6159=CARTESIAN_POINT('Ctrl Pts',(0.319651197590554,0.113548934374436,1.71233030884879));
#6160=CARTESIAN_POINT('Ctrl Pts',(0.210918141794392,0.266931928573215,1.72652079296202));
#6161=CARTESIAN_POINT('Ctrl Pts',(0.0367565960986196,0.33914953789685,1.74075114688302));
#6162=CARTESIAN_POINT('Ctrl Pts',(-0.149685558776009,0.307602531834638,
1.75501873521155));
#6163=CARTESIAN_POINT('Ctrl Pts',(-0.290952593298896,0.181283052059042,
1.76932343108276));
#6164=CARTESIAN_POINT('Ctrl Pts',(-0.343624299509979,-0.00122470576221222,
1.78366073529875));
#6165=CARTESIAN_POINT('Ctrl Pts',(-0.290980868645007,-0.184182288319934,
1.79802970310735));
#6166=CARTESIAN_POINT('Ctrl Pts',(-0.148771903912068,-0.311336659778199,
1.81242794870657));
#6167=CARTESIAN_POINT('Ctrl Pts',(0.03964924936428,-0.343404204343566,1.82685321116496));
#6168=CARTESIAN_POINT('Ctrl Pts',(0.216555130910507,-0.270158948781549,
1.84130317466462));
#6169=CARTESIAN_POINT('Ctrl Pts',(0.327545313208071,-0.113818423308632,
1.85577536070366));
#6170=CARTESIAN_POINT('Ctrl Pts',(0.338363125822719,0.0779740906565071,
1.87026757403339));
#6171=CARTESIAN_POINT('Ctrl Pts',(0.245361396637451,0.246111297670799,1.88477684497455));
#6172=CARTESIAN_POINT('Ctrl Pts',(0.0583067834553886,0.349974365607058,
1.90091574842115));
#6173=CARTESIAN_POINT('Ctrl Pts',(-0.181787851399422,0.314354426222109,
1.91868303616071));
#6174=CARTESIAN_POINT('Ctrl Pts',(-0.346789882068873,0.106664965971596,
1.93808521951499));
#6175=CARTESIAN_POINT('Ctrl Pts',(-0.330496339658479,-0.113422069416505,
1.9542610714215));
#6176=CARTESIAN_POINT('Ctrl Pts',(-0.230283779721878,-0.248105619725249,
1.96720310592885));
#6177=CARTESIAN_POINT('Ctrl Pts',(-0.0883522547555857,-0.337843644550113,
1.98014846800894));
#6178=CARTESIAN_POINT('Ctrl Pts',(0.0659064686942833,-0.337971037882213,
1.99146805063414));
#6179=CARTESIAN_POINT('Ctrl Pts',(0.176715751168689,-0.281702711275593,
2.00117298579014));
#6180=CARTESIAN_POINT('Ctrl Pts',(0.242310061646865,-0.231388071089323,
2.00764183259477));
#6181=CARTESIAN_POINT('Ctrl Pts',(0.329896261130398,-0.113455911595648,
2.01895911802151));
#6182=CARTESIAN_POINT('Ctrl Pts',(0.346963705804559,0.106219379641946,2.03511657263834));
#6183=CARTESIAN_POINT('Ctrl Pts',(0.181421017200114,0.313529381253331,2.05448291591772));
#6184=CARTESIAN_POINT('Ctrl Pts',(-0.0578316111487914,0.349111887104915,
2.07221137618884));
#6185=CARTESIAN_POINT('Ctrl Pts',(-0.244497621198263,0.245521434385232,
2.08830552097745));
#6186=CARTESIAN_POINT('Ctrl Pts',(-0.337158982464816,0.0779154827919484,
2.1027691197373));
#6187=CARTESIAN_POINT('Ctrl Pts',(-0.326396740207177,-0.113196561520307,
2.11720948839641));
#6188=CARTESIAN_POINT('Ctrl Pts',(-0.215834447915981,-0.268925810611374,
2.1316241607543));
#6189=CARTESIAN_POINT('Ctrl Pts',(-0.0397023314431912,-0.341839636870502,
2.14601087914839));
#6190=CARTESIAN_POINT('Ctrl Pts',(0.147810528969888,-0.309966423960966,
2.16036733775139));
#6191=CARTESIAN_POINT('Ctrl Pts',(0.289279140671208,-0.183404826055055,
2.17469136125443));
#6192=CARTESIAN_POINT('Ctrl Pts',(0.32413793905981,-0.0622550446484658,
2.18421850306274));
#6193=CARTESIAN_POINT('Ctrl Pts',(0.324146149699815,-0.00148870109147552,
2.18897542715673));
#6194=CARTESIAN_POINT('Ctrl Pts',(0.284351574566012,0.00209289635755192,
1.4032377180594));
#6195=CARTESIAN_POINT('Ctrl Pts',(0.284344357328317,0.0555070994772719,
1.40741910026758));
#6196=CARTESIAN_POINT('Ctrl Pts',(0.253735841667482,0.161879987588016,1.41578500995075));
#6197=CARTESIAN_POINT('Ctrl Pts',(0.129255560771724,0.273321780593359,1.42839424570576));
#6198=CARTESIAN_POINT('Ctrl Pts',(-0.0361050419550946,0.301460299900524,
1.44105512584986));
#6199=CARTESIAN_POINT('Ctrl Pts',(-0.19180454726181,0.237074994443535,1.45377239878429));
#6200=CARTESIAN_POINT('Ctrl Pts',(-0.289812564223684,0.0991093413318229,
1.46654521640033));
#6201=CARTESIAN_POINT('Ctrl Pts',(-0.299447123537825,-0.070638578082909,
1.47937536902017));
#6202=CARTESIAN_POINT('Ctrl Pts',(-0.23755772335888,-0.182718163461684,
1.4890408587334));
#6203=CARTESIAN_POINT('Ctrl Pts',(-0.175208552710509,-0.236773567523899,
1.49550315164272));
#6204=CARTESIAN_POINT('Ctrl Pts',(-0.140568379573528,-0.259263236852212,
1.49873794667775));
#6205=CARTESIAN_POINT('Ctrl Pts',(-0.103053036763,-0.276644990895967,1.50197640326238));
#6206=CARTESIAN_POINT('Ctrl Pts',(-0.00628337548740407,-0.306213143561888,
1.50990159030283));
#6207=CARTESIAN_POINT('Ctrl Pts',(0.16466851405336,-0.280921166762252,1.52255426313202));
#6208=CARTESIAN_POINT('Ctrl Pts',(0.313343496448229,-0.094270090403481,
1.54001286072801));
#6209=CARTESIAN_POINT('Ctrl Pts',(0.297341035202232,0.124810650260335,1.55611362339848));
#6210=CARTESIAN_POINT('Ctrl Pts',(0.166930423314896,0.270157693737924,1.57082805896355));
#6211=CARTESIAN_POINT('Ctrl Pts',(-0.0021871479333846,0.319077064365966,
1.5841307898054));
#6212=CARTESIAN_POINT('Ctrl Pts',(-0.172445457813514,0.270153484695753,
1.5974930126463));
#6213=CARTESIAN_POINT('Ctrl Pts',(-0.290977247976819,0.137641678545292,
1.61091447749511));
#6214=CARTESIAN_POINT('Ctrl Pts',(-0.321026877647783,-0.038416870033602,
1.62439476923727));
#6215=CARTESIAN_POINT('Ctrl Pts',(-0.252480754699545,-0.204171031652774,
1.63793338359126));
#6216=CARTESIAN_POINT('Ctrl Pts',(-0.105644078858064,-0.30849214717115,
1.65152969033013));
#6217=CARTESIAN_POINT('Ctrl Pts',(0.0749472165069855,-0.318734659244124,
1.6651829598536));
#6218=CARTESIAN_POINT('Ctrl Pts',(0.233943323856699,-0.230950878459999,
1.67889234706262));
#6219=CARTESIAN_POINT('Ctrl Pts',(0.322332463437095,-0.0714702251109403,
1.69265670983326));
#6220=CARTESIAN_POINT('Ctrl Pts',(0.312110574480096,0.111369019946347,1.70647544116127));
#6221=CARTESIAN_POINT('Ctrl Pts',(0.205845454912002,0.261304060772099,1.72034700838273));
#6222=CARTESIAN_POINT('Ctrl Pts',(0.0354650074486262,0.331979400056782,
1.73427018684545));
#6223=CARTESIAN_POINT('Ctrl Pts',(-0.14711797487682,0.301106817491115,1.74824389266385));
#6224=CARTESIAN_POINT('Ctrl Pts',(-0.28560490328058,0.177309272695843,1.76226588379689));
#6225=CARTESIAN_POINT('Ctrl Pts',(-0.337309662661643,-0.00176488184415049,
1.77633558452815));
#6226=CARTESIAN_POINT('Ctrl Pts',(-0.285626419421087,-0.181478411719522,
1.79045084345521));
#6227=CARTESIAN_POINT('Ctrl Pts',(-0.145813563718198,-0.306526186142243,
1.80460998723798));
#6228=CARTESIAN_POINT('Ctrl Pts',(0.0396526632860302,-0.338118913343718,
1.81881118880055));
#6229=CARTESIAN_POINT('Ctrl Pts',(0.213993052827738,-0.265966707712057,
1.83305253571127));
#6230=CARTESIAN_POINT('Ctrl Pts',(0.323513667978463,-0.111746358162693,
1.84733208863259));
#6231=CARTESIAN_POINT('Ctrl Pts',(0.334229113099525,0.0776825567486598,
1.86164769315016));
#6232=CARTESIAN_POINT('Ctrl Pts',(0.242289928018038,0.243955698081078,1.87599744953428));
#6233=CARTESIAN_POINT('Ctrl Pts',(0.0571271931439024,0.346811227773582,
1.89197656081854));
#6234=CARTESIAN_POINT('Ctrl Pts',(-0.180921437098845,0.311556741369201,
1.90959711440866));
#6235=CARTESIAN_POINT('Ctrl Pts',(-0.344833685733874,0.105378317315944,
1.92886497432744));
#6236=CARTESIAN_POINT('Ctrl Pts',(-0.328686048836367,-0.11353363448047,
1.94495640357339));
#6237=CARTESIAN_POINT('Ctrl Pts',(-0.228894216428349,-0.247673192303685,
1.95784757972856));
#6238=CARTESIAN_POINT('Ctrl Pts',(-0.0874628865303489,-0.337117355536019,
1.97074826183704));
#6239=CARTESIAN_POINT('Ctrl Pts',(0.0665148567815164,-0.337289314963655,
1.98205225693581));
#6240=CARTESIAN_POINT('Ctrl Pts',(0.177201780714138,-0.281087394194614,
1.9917465206046));
#6241=CARTESIAN_POINT('Ctrl Pts',(0.24275024614819,-0.230808651930823,1.99821132889996));
#6242=CARTESIAN_POINT('Ctrl Pts',(0.330344232191523,-0.112890571889901,
2.009529543392));
#6243=CARTESIAN_POINT('Ctrl Pts',(0.347492403924234,0.10704864474084,2.02570982435864));
#6244=CARTESIAN_POINT('Ctrl Pts',(0.181535655882207,0.3150304141917,2.04513839975171));
#6245=CARTESIAN_POINT('Ctrl Pts',(-0.0588091737727422,0.350847169159054,
2.06295250484409));
#6246=CARTESIAN_POINT('Ctrl Pts',(-0.246611289832875,0.246670966545805,
2.07914587119244));
#6247=CARTESIAN_POINT('Ctrl Pts',(-0.339969156119851,0.0778684416628693,
2.09371690120608));
#6248=CARTESIAN_POINT('Ctrl Pts',(-0.329145769048135,-0.114860699832476,
2.10828205463687));
#6249=CARTESIAN_POINT('Ctrl Pts',(-0.217536412770799,-0.272112506388316,
2.12283904951299));
#6250=CARTESIAN_POINT('Ctrl Pts',(-0.0394980503574506,-0.345849044433683,
2.13738466058146));
#6251=CARTESIAN_POINT('Ctrl Pts',(0.150291350431643,-0.313616322822559,
2.15191771714466));
#6252=CARTESIAN_POINT('Ctrl Pts',(0.293659717677233,-0.185414557532162,
2.16643262471795));
#6253=CARTESIAN_POINT('Ctrl Pts',(0.329066204710721,-0.0625058077220191,
2.17610149040741));
#6254=CARTESIAN_POINT('Ctrl Pts',(0.329074534271164,-0.000859342736721239,
2.18092731235806));
#6255=CARTESIAN_POINT('Ctrl Pts',(0.271492587378726,0.00109723241378548,
1.41593442625805));
#6256=CARTESIAN_POINT('Ctrl Pts',(0.271485694290624,0.052112430132334,1.41992800900624));
#6257=CARTESIAN_POINT('Ctrl Pts',(0.242249559139038,0.153586730774769,1.42791007606117));
#6258=CARTESIAN_POINT('Ctrl Pts',(0.123659626324257,0.259706097017051,1.43992072996988));
#6259=CARTESIAN_POINT('Ctrl Pts',(-0.0335930623853517,0.286428140373609,
1.45196090010097));
#6260=CARTESIAN_POINT('Ctrl Pts',(-0.18141482672022,0.225267890136344,1.4640363624814));
#6261=CARTESIAN_POINT('Ctrl Pts',(-0.274318874126518,0.094438252948025,
1.47614773226753));
#6262=CARTESIAN_POINT('Ctrl Pts',(-0.283417169160825,-0.0663035653041664,
1.48829769185157));
#6263=CARTESIAN_POINT('Ctrl Pts',(-0.224864636858723,-0.172308199765865,
1.49744065450877));
#6264=CARTESIAN_POINT('Ctrl Pts',(-0.16593170165895,-0.223401513993078,
1.50354898148737));
#6265=CARTESIAN_POINT('Ctrl Pts',(-0.133197290901991,-0.244653576577957,
1.50660582486713));
#6266=CARTESIAN_POINT('Ctrl Pts',(-0.097754906384767,-0.261074677072147,
1.50966538240655));
#6267=CARTESIAN_POINT('Ctrl Pts',(-0.00635215241037408,-0.289001855159658,
1.51715100459395));
#6268=CARTESIAN_POINT('Ctrl Pts',(0.155004993833741,-0.265095701696411,
1.52909474424491));
#6269=CARTESIAN_POINT('Ctrl Pts',(0.295165120037499,-0.0890774075493339,
1.54555712282203));
#6270=CARTESIAN_POINT('Ctrl Pts',(0.280063643211613,0.11733841973294,1.56072753588602));
#6271=CARTESIAN_POINT('Ctrl Pts',(0.157246215363437,0.254211665897086,1.57458501593487));
#6272=CARTESIAN_POINT('Ctrl Pts',(-0.00197270028535737,0.300263721233418,
1.5871091434798));
#6273=CARTESIAN_POINT('Ctrl Pts',(-0.162235754907892,0.254210796053949,
1.59968706600409));
#6274=CARTESIAN_POINT('Ctrl Pts',(-0.273804433807857,0.129485742602018,
1.61231997991121));
#6275=CARTESIAN_POINT('Ctrl Pts',(-0.302094559974484,-0.0362384831563508,
1.62500901828759));
#6276=CARTESIAN_POINT('Ctrl Pts',(-0.237566582128313,-0.192294748298478,
1.63775518726396));
#6277=CARTESIAN_POINT('Ctrl Pts',(-0.0992882607141231,-0.290547628373896,
1.65055939320127));
#6278=CARTESIAN_POINT('Ctrl Pts',(0.0708532123640876,-0.300210016777284,
1.66342242123036));
#6279=CARTESIAN_POINT('Ctrl Pts',(0.220734377664724,-0.217475815836061,
1.67634494789799));
#6280=CARTESIAN_POINT('Ctrl Pts',(0.304120921236133,-0.0670576746065354,
1.6893276806875));
#6281=CARTESIAN_POINT('Ctrl Pts',(0.294493037088311,0.105526319670907,1.70237071363371));
#6282=CARTESIAN_POINT('Ctrl Pts',(0.194123591577484,0.247183982583743,1.71547466227991));
#6283=CARTESIAN_POINT('Ctrl Pts',(0.0330240595431114,0.314036071305745,
1.72863970901699));
#6284=CARTESIAN_POINT('Ctrl Pts',(-0.139805002589633,0.284842603775967,
1.74186572143678));
#6285=CARTESIAN_POINT('Ctrl Pts',(-0.271061350072721,0.167547140942527,
1.75515329680073));
#6286=CARTESIAN_POINT('Ctrl Pts',(-0.320149825119423,-0.0023451892674139,
1.76850151258264));
#6287=CARTESIAN_POINT('Ctrl Pts',(-0.271083065196151,-0.173086876640925,
1.78191051150415));
#6288=CARTESIAN_POINT('Ctrl Pts',(-0.138097485184967,-0.292077909506515,
1.79537986457642));
#6289=CARTESIAN_POINT('Ctrl Pts',(0.0385983399591338,-0.32221636504151,
1.80890908708627));
#6290=CARTESIAN_POINT('Ctrl Pts',(0.204974200986741,-0.253404878031692,
1.82249757886881));
#6291=CARTESIAN_POINT('Ctrl Pts',(0.30968647607717,-0.106029489164137,1.83614458498297));
#6292=CARTESIAN_POINT('Ctrl Pts',(0.319991027068231,0.0753271207673322,
1.84984935113891));
#6293=CARTESIAN_POINT('Ctrl Pts',(0.231853242034047,0.234821776128565,1.86361075588294));
#6294=CARTESIAN_POINT('Ctrl Pts',(0.0539694368211627,0.333696079427026,
1.87896342144752));
#6295=CARTESIAN_POINT('Ctrl Pts',(-0.175267053549315,0.299865670659702,
1.89592802781899));
#6296=CARTESIAN_POINT('Ctrl Pts',(-0.333627242296529,0.100875417751075,
1.91453010909236));
#6297=CARTESIAN_POINT('Ctrl Pts',(-0.318103980909791,-0.111059428495346,
1.9301070109208));
#6298=CARTESIAN_POINT('Ctrl Pts',(-0.221308531106851,-0.241211547793202,
1.94261179799545));
#6299=CARTESIAN_POINT('Ctrl Pts',(-0.0839111034095029,-0.328129409655272,
1.95514599042185));
#6300=CARTESIAN_POINT('Ctrl Pts',(0.0659787415594033,-0.328371864806453,
1.96614735699824));
#6301=CARTESIAN_POINT('Ctrl Pts',(0.173954717379698,-0.273553446450119,
1.97560349817015));
#6302=CARTESIAN_POINT('Ctrl Pts',(0.237941925838186,-0.224474378223391,
1.98191395714428));
#6303=CARTESIAN_POINT('Ctrl Pts',(0.323555514713298,-0.10925931253578,1.99297373967346));
#6304=CARTESIAN_POINT('Ctrl Pts',(0.340469789748638,0.106136096135639,2.00881942885412));
#6305=CARTESIAN_POINT('Ctrl Pts',(0.177559260022394,0.310550581792306,2.02790293557778));
#6306=CARTESIAN_POINT('Ctrl Pts',(-0.0592704015937349,0.345982341429199,
2.0454553049926));
#6307=CARTESIAN_POINT('Ctrl Pts',(-0.244890194023234,0.243100762578732,
2.06145549117311));
#6308=CARTESIAN_POINT('Ctrl Pts',(-0.337416126210674,0.0759330719099003,
2.07588653464397));
#6309=CARTESIAN_POINT('Ctrl Pts',(-0.326737063233083,-0.115421783027243,
2.09034610228147));
#6310=CARTESIAN_POINT('Ctrl Pts',(-0.215715969562994,-0.271959300347246,
2.10483205671323));
#6311=CARTESIAN_POINT('Ctrl Pts',(-0.0381314606062155,-0.345579124738108,
2.1193413423825));
#6312=CARTESIAN_POINT('Ctrl Pts',(0.151660986646548,-0.313406934885558,
2.13387292093976));
#6313=CARTESIAN_POINT('Ctrl Pts',(0.295411443757773,-0.184948656073821,
2.14842109049688));
#6314=CARTESIAN_POINT('Ctrl Pts',(0.331011968991107,-0.0614504945185775,
2.15813557967852));
#6315=CARTESIAN_POINT('Ctrl Pts',(0.331020345667048,0.000544668811153922,
2.16298869850864));
#6316=CARTESIAN_POINT('Ctrl Pts',(0.266533420052219,-0.000598446861652248,
1.43758697109781));
#6317=CARTESIAN_POINT('Ctrl Pts',(0.26652665376501,0.0494783075173114,1.44150709042139));
#6318=CARTESIAN_POINT('Ctrl Pts',(0.237828564223823,0.148934102677714,1.44933094401217));
#6319=CARTESIAN_POINT('Ctrl Pts',(0.121941169632728,0.252533932703974,1.46106241271628));
#6320=CARTESIAN_POINT('Ctrl Pts',(-0.031148631117057,0.278475984569276,
1.47278278595574));
#6321=CARTESIAN_POINT('Ctrl Pts',(-0.174537915324736,0.219070557052679,
1.4844981379325));
#6322=CARTESIAN_POINT('Ctrl Pts',(-0.264320512406116,0.0925130070182829,
1.49620987741958));
#6323=CARTESIAN_POINT('Ctrl Pts',(-0.273019793758845,-0.0624384219482381,
1.50792159815808));
#6324=CARTESIAN_POINT('Ctrl Pts',(-0.216708588582917,-0.164278737895499,
1.51670721227717));
#6325=CARTESIAN_POINT('Ctrl Pts',(-0.160180892291219,-0.213283628024979,
1.52256612937649));
#6326=CARTESIAN_POINT('Ctrl Pts',(-0.128805227872014,-0.233652238038377,
1.5254959752123));
#6327=CARTESIAN_POINT('Ctrl Pts',(-0.0948602906438099,-0.249378490854682,
1.5284262570081));
#6328=CARTESIAN_POINT('Ctrl Pts',(-0.0073795378077737,-0.27610445683934,
1.53559033771115));
#6329=CARTESIAN_POINT('Ctrl Pts',(0.146673956766819,-0.253167685233027,
1.54699409155007));
#6330=CARTESIAN_POINT('Ctrl Pts',(0.279896500835626,-0.0856285728439146,
1.56265532418908));
#6331=CARTESIAN_POINT('Ctrl Pts',(0.265458901440563,0.110056712248341,1.57703752301133));
#6332=CARTESIAN_POINT('Ctrl Pts',(0.149308581978497,0.239404593439139,1.59013780265147));
#6333=CARTESIAN_POINT('Ctrl Pts',(-0.000879246359104834,0.282794954861585,
1.60195050522868));
#6334=CARTESIAN_POINT('Ctrl Pts',(-0.15169922660277,0.239404889893613,1.61378836786326));
#6335=CARTESIAN_POINT('Ctrl Pts',(-0.256457774506062,0.122226885907837,
1.62565404553147));
#6336=CARTESIAN_POINT('Ctrl Pts',(-0.282939238014729,-0.0331463294577391,
1.63755013589437));
#6337=CARTESIAN_POINT('Ctrl Pts',(-0.222513907990111,-0.179181116194557,
1.6494791816529));
#6338=CARTESIAN_POINT('Ctrl Pts',(-0.0932867834705937,-0.270960294371653,
1.66144366426743));
#6339=CARTESIAN_POINT('Ctrl Pts',(0.0654677283059359,-0.279944637602497,
1.67344599120345));
#6340=CARTESIAN_POINT('Ctrl Pts',(0.205124760040014,-0.202822617250478,
1.68548851375222));
#6341=CARTESIAN_POINT('Ctrl Pts',(0.282720976254736,-0.0627985050799433,
1.69757329221837));
#6342=CARTESIAN_POINT('Ctrl Pts',(0.273746547884209,0.0976912909106923,
1.70970294432419));
#6343=CARTESIAN_POINT('Ctrl Pts',(0.180471658752939,0.229304408207884,1.72187920671603));
#6344=CARTESIAN_POINT('Ctrl Pts',(0.0308764741788442,0.291367908294201,
1.73410415425347));
#6345=CARTESIAN_POINT('Ctrl Pts',(-0.129523158214965,0.264262077447812,
1.74637987496184));
#6346=CARTESIAN_POINT('Ctrl Pts',(-0.251291518773948,0.155437729951258,
1.75870764348809));
#6347=CARTESIAN_POINT('Ctrl Pts',(-0.296820627951342,-0.00215178387272073,
1.77108984108917));
#6348=CARTESIAN_POINT('Ctrl Pts',(-0.251309762852418,-0.160519102576093,
1.78352773391814));
#6349=CARTESIAN_POINT('Ctrl Pts',(-0.127952255814083,-0.270899775685238,
1.79602286205806));
#6350=CARTESIAN_POINT('Ctrl Pts',(0.0359923471661857,-0.298870254746358,
1.8085766053069));
#6351=CARTESIAN_POINT('Ctrl Pts',(0.190426644024177,-0.235008880970683,
1.82119023321984));
#6352=CARTESIAN_POINT('Ctrl Pts',(0.287682855256994,-0.0981507875079271,
1.83386492806554));
#6353=CARTESIAN_POINT('Ctrl Pts',(0.297276612211721,0.0703845270426061,
1.84660167249208));
#6354=CARTESIAN_POINT('Ctrl Pts',(0.215320379043628,0.218732235998905,1.85940151393512));
#6355=CARTESIAN_POINT('Ctrl Pts',(0.0497410880640545,0.310798493864736,
1.87369422624341));
#6356=CARTESIAN_POINT('Ctrl Pts',(-0.163934573054978,0.279322056893055,
1.88950895549613));
#6357=CARTESIAN_POINT('Ctrl Pts',(-0.311842090402094,0.093597039791909,
1.90687638344953));
#6358=CARTESIAN_POINT('Ctrl Pts',(-0.297389946716595,-0.104635041214907,
1.92144675642255));
#6359=CARTESIAN_POINT('Ctrl Pts',(-0.206725724713414,-0.226570099612231,
1.9331617974391));
#6360=CARTESIAN_POINT('Ctrl Pts',(-0.0778995181755873,-0.308087964657102,
1.94491517743614));
#6361=CARTESIAN_POINT('Ctrl Pts',(0.0629117092812275,-0.308372369450851,
1.95525227591192));
#6362=CARTESIAN_POINT('Ctrl Pts',(0.164490964977537,-0.256807355278177,
1.96414796506574));
#6363=CARTESIAN_POINT('Ctrl Pts',(0.224722944339505,-0.21060994633766,1.97008821946209));
#6364=CARTESIAN_POINT('Ctrl Pts',(0.305401073256525,-0.10206812301548,1.98050932509365));
#6365=CARTESIAN_POINT('Ctrl Pts',(0.321462965061058,0.101261332430962,1.99546946518584));
#6366=CARTESIAN_POINT('Ctrl Pts',(0.167353833457747,0.294860683101063,2.01353713913069));
#6367=CARTESIAN_POINT('Ctrl Pts',(-0.0574805364540771,0.328622162338068,
2.03020314733791));
#6368=CARTESIAN_POINT('Ctrl Pts',(-0.234210607295154,0.230747071427096,
2.04543515185281));
#6369=CARTESIAN_POINT('Ctrl Pts',(-0.322547239746861,0.0712703181694491,
2.05920591331795));
#6370=CARTESIAN_POINT('Ctrl Pts',(-0.312395670542285,-0.111759879847481,
2.07303733322864));
#6371=CARTESIAN_POINT('Ctrl Pts',(-0.205992467238026,-0.26189561908817,
2.08692864153008));
#6372=CARTESIAN_POINT('Ctrl Pts',(-0.035301754120549,-0.33272882463994,
2.10087770204531));
#6373=CARTESIAN_POINT('Ctrl Pts',(0.147640705043926,-0.301785489794866,
2.11488504909042));
#6374=CARTESIAN_POINT('Ctrl Pts',(0.286610389683,-0.177698918117886,2.12894498467352));
#6375=CARTESIAN_POINT('Ctrl Pts',(0.321161806690122,-0.0580367709741704,
2.13835992180599));
#6376=CARTESIAN_POINT('Ctrl Pts',(0.32116993299807,0.00210543722720802,
2.14306798720062));
#6377=CARTESIAN_POINT('Ctrl Pts',(0.285097284651427,-0.00241889983639149,
1.46087401350103));
#6378=CARTESIAN_POINT('Ctrl Pts',(0.285090059199041,0.0510560995578562,
1.46506015497633));
#6379=CARTESIAN_POINT('Ctrl Pts',(0.254405463959297,0.157243204973338,1.47341492833332));
#6380=CARTESIAN_POINT('Ctrl Pts',(0.131112493365165,0.267329197540611,1.48588887820255));
#6381=CARTESIAN_POINT('Ctrl Pts',(-0.0310790590612892,0.294737110561081,
1.49830621261202));
#6382=CARTESIAN_POINT('Ctrl Pts',(-0.182346981068028,0.231966474128732,
1.51066809926437));
#6383=CARTESIAN_POINT('Ctrl Pts',(-0.276622840120502,0.0989160846808463,
1.52297638590209));
#6384=CARTESIAN_POINT('Ctrl Pts',(-0.28562935546202,-0.0632450379079678,
1.53523274919662));
#6385=CARTESIAN_POINT('Ctrl Pts',(-0.226890031412833,-0.169325517012616,
1.54438751719497));
#6386=CARTESIAN_POINT('Ctrl Pts',(-0.168150306427595,-0.220243786261342,
1.55047565341104));
#6387=CARTESIAN_POINT('Ctrl Pts',(-0.135581939101061,-0.241384906042715,
1.55351674869088));
#6388=CARTESIAN_POINT('Ctrl Pts',(-0.100387654468105,-0.257688371292987,
1.55655490244068));
#6389=CARTESIAN_POINT('Ctrl Pts',(-0.0097824441123277,-0.285365009758757,
1.56397439181196));
#6390=CARTESIAN_POINT('Ctrl Pts',(0.149173126959868,-0.261514184936789,
1.5757425298963));
#6391=CARTESIAN_POINT('Ctrl Pts',(0.285602172828371,-0.0895278583518576,
1.59180512762946));
#6392=CARTESIAN_POINT('Ctrl Pts',(0.270659165239267,0.10990564271393,1.60646359224198));
#6393=CARTESIAN_POINT('Ctrl Pts',(0.152845360024874,0.240914998182156,1.61974140254765));
#6394=CARTESIAN_POINT('Ctrl Pts',(0.00132058495251339,0.284586289092117,
1.63165684771419));
#6395=CARTESIAN_POINT('Ctrl Pts',(-0.150052838385872,0.240923309697256,
1.6435401615279));
#6396=CARTESIAN_POINT('Ctrl Pts',(-0.254628743279724,0.123790276438128,
1.65539393682687));
#6397=CARTESIAN_POINT('Ctrl Pts',(-0.280852713971101,-0.0307010402102851,
1.66722078080952));
#6398=CARTESIAN_POINT('Ctrl Pts',(-0.220968814531156,-0.175151607286856,
1.67902337392248));
#6399=CARTESIAN_POINT('Ctrl Pts',(-0.0936586927728087,-0.265441896093515,
1.69080443492152));
#6400=CARTESIAN_POINT('Ctrl Pts',(0.0619320971189879,-0.274144025980544,
1.70256672698207));
#6401=CARTESIAN_POINT('Ctrl Pts',(0.198109144806248,-0.198827325563695,
1.71431302884181));
#6402=CARTESIAN_POINT('Ctrl Pts',(0.273365251138184,-0.0628212764942574,
1.72604644031572));
#6403=CARTESIAN_POINT('Ctrl Pts',(0.264591572289594,0.0922867316427776,
1.73776923268641));
#6404=CARTESIAN_POINT('Ctrl Pts',(0.174764652560144,0.218869799124979,1.74948474865086));
#6405=CARTESIAN_POINT('Ctrl Pts',(0.0314157170558157,0.278239262102867,
1.76119576873161));
#6406=CARTESIAN_POINT('Ctrl Pts',(-0.121576817067625,0.252291826805016,
1.77290499016194));
#6407=CARTESIAN_POINT('Ctrl Pts',(-0.237194160915694,0.148844679759727,
1.7846159414541));
#6408=CARTESIAN_POINT('Ctrl Pts',(-0.280189871842215,-0.000283120495965188,
1.79633073217163));
#6409=CARTESIAN_POINT('Ctrl Pts',(-0.237216648905561,-0.149519446584567,
1.80805264345696));
#6410=CARTESIAN_POINT('Ctrl Pts',(-0.121334725719892,-0.253103788167418,
1.8197845112682));
#6411=CARTESIAN_POINT('Ctrl Pts',(0.032065824366413,-0.279197448292019,
1.83152919415975));
#6412=CARTESIAN_POINT('Ctrl Pts',(0.176032876548686,-0.219585186162864,
1.8432895314691));
#6413=CARTESIAN_POINT('Ctrl Pts',(0.266363672526068,-0.0923525264685545,
1.85506830270555));
#6414=CARTESIAN_POINT('Ctrl Pts',(0.275185263312216,0.0638000977606677,
1.86686833472312));
#6415=CARTESIAN_POINT('Ctrl Pts',(0.19942055667018,0.200817401186163,1.87869222140788));
#6416=CARTESIAN_POINT('Ctrl Pts',(0.0468336660220393,0.285581780166665,
1.89185969859235));
#6417=CARTESIAN_POINT('Ctrl Pts',(-0.149427870647855,0.256552776774109,
1.90638482005989));
#6418=CARTESIAN_POINT('Ctrl Pts',(-0.284785839872206,0.0863936580923987,
1.92228945474259));
#6419=CARTESIAN_POINT('Ctrl Pts',(-0.271505592195012,-0.0946541618773216,
1.93559641358745));
#6420=CARTESIAN_POINT('Ctrl Pts',(-0.18883448665128,-0.205814296251183,
1.94627666316605));
#6421=CARTESIAN_POINT('Ctrl Pts',(-0.0714878972225447,-0.280048650077599,
1.95698178449418));
#6422=CARTESIAN_POINT('Ctrl Pts',(0.056557422971355,-0.280266379011788,
1.96638001843711));
#6423=CARTESIAN_POINT('Ctrl Pts',(0.148842638659517,-0.233416525658896,
1.97446193547615));
#6424=CARTESIAN_POINT('Ctrl Pts',(0.203544042920288,-0.191460234672681,
1.97985660168861));
#6425=CARTESIAN_POINT('Ctrl Pts',(0.276766158498589,-0.0929323996780253,
1.9893151942404));
#6426=CARTESIAN_POINT('Ctrl Pts',(0.291296648239029,0.0914545316801896,
2.002880442837));
#6427=CARTESIAN_POINT('Ctrl Pts',(0.151649974014536,0.266828988428087,2.01924800893444));
#6428=CARTESIAN_POINT('Ctrl Pts',(-0.051938403746315,0.297387291798137,
2.03433788910338));
#6429=CARTESIAN_POINT('Ctrl Pts',(-0.211943418815992,0.20877346918723,2.04812762550537));
#6430=CARTESIAN_POINT('Ctrl Pts',(-0.291927406141446,0.0643829424248649,
2.06059498063548));
#6431=CARTESIAN_POINT('Ctrl Pts',(-0.282742302054825,-0.101374482622084,
2.0731204043778));
#6432=CARTESIAN_POINT('Ctrl Pts',(-0.18634967584022,-0.237409536214224,
2.08570530126253));
#6433=CARTESIAN_POINT('Ctrl Pts',(-0.0316120397930279,-0.301638279150675,
2.09835073112393));
#6434=CARTESIAN_POINT('Ctrl Pts',(0.13437413324299,-0.27359223176401,2.11105823551128));
#6435=CARTESIAN_POINT('Ctrl Pts',(0.260600324022261,-0.160901490961837,
2.1238278967204));
#6436=CARTESIAN_POINT('Ctrl Pts',(0.292024278813734,-0.0521464631533842,
2.13238426955925));
#6437=CARTESIAN_POINT('Ctrl Pts',(0.292031677431713,0.00261016504483008,
2.13667073981128));
#6438=CARTESIAN_POINT('Ctrl Pts',(0.314888635514893,-0.00241091183326431,
1.46082339350253));
#6439=CARTESIAN_POINT('Ctrl Pts',(0.31488066604922,0.0565704708297952,1.46544058686453));
#6440=CARTESIAN_POINT('Ctrl Pts',(0.281007406696283,0.173862408081188,1.47466873695446));
#6441=CARTESIAN_POINT('Ctrl Pts',(0.144847554197953,0.295426491012178,1.48844337668646));
#6442=CARTESIAN_POINT('Ctrl Pts',(-0.0342851373916114,0.325706577815792,
1.50215841582855));
#6443=CARTESIAN_POINT('Ctrl Pts',(-0.201331441874071,0.256378388746261,
1.51580959638849));
#6444=CARTESIAN_POINT('Ctrl Pts',(-0.305399495530267,0.109489858454975,
1.52939761607679));
#6445=CARTESIAN_POINT('Ctrl Pts',(-0.315320196692728,-0.0694407339097994,
1.54292114176174));
#6446=CARTESIAN_POINT('Ctrl Pts',(-0.250539306529347,-0.18639704075144,
1.55301514961419));
#6447=CARTESIAN_POINT('Ctrl Pts',(-0.18580905138686,-0.242506716265914,
1.55972411928833));
#6448=CARTESIAN_POINT('Ctrl Pts',(-0.149927816391745,-0.265797847575212,
1.56307451809262));
#6449=CARTESIAN_POINT('Ctrl Pts',(-0.111163875464346,-0.283754347820401,
1.566420820712));
#6450=CARTESIAN_POINT('Ctrl Pts',(-0.011394113389426,-0.314229695144002,
1.57459065039502));
#6451=CARTESIAN_POINT('Ctrl Pts',(0.163474807395259,-0.28793328486503,1.5875374009987));
#6452=CARTESIAN_POINT('Ctrl Pts',(0.313213210997328,-0.0990169221446236,
1.60517584236345));
#6453=CARTESIAN_POINT('Ctrl Pts',(0.296744609610656,0.119492548342282,1.62123688662316));
#6454=CARTESIAN_POINT('Ctrl Pts',(0.167905869182534,0.262670401766488,1.63575254694344));
#6455=CARTESIAN_POINT('Ctrl Pts',(0.00259435741764641,0.310260621883403,
1.64875115909385));
#6456=CARTESIAN_POINT('Ctrl Pts',(-0.162138978273715,0.262681198120579,
1.66168469519045));
#6457=CARTESIAN_POINT('Ctrl Pts',(-0.275621710656057,0.135476363579829,
1.67455370237198));
#6458=CARTESIAN_POINT('Ctrl Pts',(-0.303947788371616,-0.0318025544323174,
1.68735884399675));
#6459=CARTESIAN_POINT('Ctrl Pts',(-0.239232326675737,-0.187720156696059,
1.70010091014339));
#6460=CARTESIAN_POINT('Ctrl Pts',(-0.102168915306409,-0.284835237870766,
1.71278081298448));
#6461=CARTESIAN_POINT('Ctrl Pts',(0.0647507693491276,-0.294091793930313,
1.72539958234459));
#6462=CARTESIAN_POINT('Ctrl Pts',(0.210302405961457,-0.213496390348748,
1.7379583760209));
#6463=CARTESIAN_POINT('Ctrl Pts',(0.290399378819606,-0.0685648846902543,
1.75045830668886));
#6464=CARTESIAN_POINT('Ctrl Pts',(0.280997576102868,0.0960562826133116,
1.76290109090414));
#6465=CARTESIAN_POINT('Ctrl Pts',(0.185951839499003,0.229833807773724,1.77528794274805));
#6466=CARTESIAN_POINT('Ctrl Pts',(0.0349645157607975,0.292265615993788,
1.78762050889942));
#6467=CARTESIAN_POINT('Ctrl Pts',(-0.125462570041385,0.26495688981232,1.79990064341502));
#6468=CARTESIAN_POINT('Ctrl Pts',(-0.246125469550108,0.156864561640384,
1.81212970168938));
#6469=CARTESIAN_POINT('Ctrl Pts',(-0.290730578144321,0.00178869821857768,
1.82431014291597));
#6470=CARTESIAN_POINT('Ctrl Pts',(-0.246152133523863,-0.152651683052016,
1.83644367698913));
#6471=CARTESIAN_POINT('Ctrl Pts',(-0.126682433121871,-0.25930391813005,
1.84853242569022));
#6472=CARTESIAN_POINT('Ctrl Pts',(0.0306642005710787,-0.285962041058737,
1.86057855192037));
#6473=CARTESIAN_POINT('Ctrl Pts',(0.177586179060693,-0.225011410333218,
1.87258430463161));
#6474=CARTESIAN_POINT('Ctrl Pts',(0.26927399222783,-0.095683591155606,1.88455203531386));
#6475=CARTESIAN_POINT('Ctrl Pts',(0.278084925824305,0.0622130540219098,
1.8964840977736));
#6476=CARTESIAN_POINT('Ctrl Pts',(0.201753576721663,0.200038156901172,1.90838307166345));
#6477=CARTESIAN_POINT('Ctrl Pts',(0.0488818383881024,0.284820769561344,
1.92156992514232));
#6478=CARTESIAN_POINT('Ctrl Pts',(-0.146535093892137,0.25567223899667,1.93603617489917));
#6479=CARTESIAN_POINT('Ctrl Pts',(-0.280249802687413,0.0871596115803118,
1.9517731940105));
#6480=CARTESIAN_POINT('Ctrl Pts',(-0.266987101998673,-0.090825328261591,
1.96485665128121));
#6481=CARTESIAN_POINT('Ctrl Pts',(-0.186064361045936,-0.199562543379855,
1.97530826657453));
#6482=CARTESIAN_POINT('Ctrl Pts',(-0.0715738890859495,-0.27194086119468,
1.98575016408737));
#6483=CARTESIAN_POINT('Ctrl Pts',(0.0527681653931571,-0.272020816451964,
1.99487777982029));
#6484=CARTESIAN_POINT('Ctrl Pts',(0.142020233979434,-0.226699224433259,
2.00269503679117));
#6485=CARTESIAN_POINT('Ctrl Pts',(0.194849199560625,-0.186175829667411,
2.00790531695633));
#6486=CARTESIAN_POINT('Ctrl Pts',(0.26538453361425,-0.0912003750099694,
2.01702045742602));
#6487=CARTESIAN_POINT('Ctrl Pts',(0.279140342627061,0.0857273504720853,
2.03003586593044));
#6488=CARTESIAN_POINT('Ctrl Pts',(0.145738477869324,0.25287900544541,2.04565135075897));
#6489=CARTESIAN_POINT('Ctrl Pts',(-0.0474301726531468,0.281679315861089,
2.05996861217462));
#6490=CARTESIAN_POINT('Ctrl Pts',(-0.198476529428579,0.197914796760607,
2.07299160637881));
#6491=CARTESIAN_POINT('Ctrl Pts',(-0.273651952890791,0.0620394523940554,
2.08472102715745));
#6492=CARTESIAN_POINT('Ctrl Pts',(-0.264962198551285,-0.0933233659048604,
2.09646205614446));
#6493=CARTESIAN_POINT('Ctrl Pts',(-0.174865697747918,-0.220344133944316,
2.1082173622539));
#6494=CARTESIAN_POINT('Ctrl Pts',(-0.0307882849390207,-0.28006808447709,
2.11999016920861));
#6495=CARTESIAN_POINT('Ctrl Pts',(0.123235668238189,-0.253987402111434,
2.13178230852711));
#6496=CARTESIAN_POINT('Ctrl Pts',(0.239978957267943,-0.14966309953415,2.14359862418644));
#6497=CARTESIAN_POINT('Ctrl Pts',(0.268938930763692,-0.0493657724660812,
2.15148951655109));
#6498=CARTESIAN_POINT('Ctrl Pts',(0.268945755514944,0.00114371023782948,
2.15544351083781));
#6499=CARTESIAN_POINT('Ctrl Pts',(0.33350426217158,-0.00059269602393798,
1.43762910263796));
#6500=CARTESIAN_POINT('Ctrl Pts',(0.33349582470557,0.0618523199636564,1.44251743689346));
#6501=CARTESIAN_POINT('Ctrl Pts',(0.29762198454481,0.186264933883794,1.45230507780882));
#6502=CARTESIAN_POINT('Ctrl Pts',(0.152822448193178,0.315652416567409,1.46695951175481));
#6503=CARTESIAN_POINT('Ctrl Pts',(-0.0383328670928585,0.348050441216263,
1.48159650359311));
#6504=CARTESIAN_POINT('Ctrl Pts',(-0.217170947159076,0.273915243990747,
1.49620901228621));
#6505=CARTESIAN_POINT('Ctrl Pts',(-0.328953907481535,0.116273487480008,
1.51079639226664));
#6506=CARTESIAN_POINT('Ctrl Pts',(-0.339710227550737,-0.0763447775316334,
1.52535497546158));
#6507=CARTESIAN_POINT('Ctrl Pts',(-0.269832110033659,-0.202616097899319,
1.53625099803897));
#6508=CARTESIAN_POINT('Ctrl Pts',(-0.199851822715115,-0.263279824833576,
1.54350421430842));
#6509=CARTESIAN_POINT('Ctrl Pts',(-0.161036601589138,-0.28847685119871,
1.54712869281073));
#6510=CARTESIAN_POINT('Ctrl Pts',(-0.119075517257528,-0.30791540642489,
1.55075099769877));
#6511=CARTESIAN_POINT('Ctrl Pts',(-0.0110145788198074,-0.340926517013328,
1.55960012258723));
#6512=CARTESIAN_POINT('Ctrl Pts',(0.178779397072994,-0.312500615344175,
1.57365122925557));
#6513=CARTESIAN_POINT('Ctrl Pts',(0.341888081512569,-0.106946886916083,
1.59285101394101));
#6514=CARTESIAN_POINT('Ctrl Pts',(0.324027764111286,0.131568208827147,1.6103821375933));
#6515=CARTESIAN_POINT('Ctrl Pts',(0.183128836209753,0.288235889823992,1.6262610920956));
#6516=CARTESIAN_POINT('Ctrl Pts',(0.00199318449518641,0.340425594849694,
1.64050492212001));
#6517=CARTESIAN_POINT('Ctrl Pts',(-0.178814710744046,0.288246874522815,
1.65469959848629));
#6518=CARTESIAN_POINT('Ctrl Pts',(-0.303564976297722,0.148465660357223,
1.66884320009202));
#6519=CARTESIAN_POINT('Ctrl Pts',(-0.334766024780997,-0.0356039414078766,
1.68293395112495));
#6520=CARTESIAN_POINT('Ctrl Pts',(-0.263501466362289,-0.207369781260881,
1.69697015402715));
#6521=CARTESIAN_POINT('Ctrl Pts',(-0.112393993862094,-0.314462369886333,
1.71095022654457));
#6522=CARTESIAN_POINT('Ctrl Pts',(0.0717736879435312,-0.324692465946504,
1.72487268877397));
#6523=CARTESIAN_POINT('Ctrl Pts',(0.232455731514219,-0.235732487197711,
1.73873617356272));
#6524=CARTESIAN_POINT('Ctrl Pts',(0.320912988717144,-0.075688900837101,
1.75253956750793));
#6525=CARTESIAN_POINT('Ctrl Pts',(0.310531286438101,0.106125972684126,1.76628140037764));
#6526=CARTESIAN_POINT('Ctrl Pts',(0.205561190534091,0.253868234028805,1.77996092667565));
#6527=CARTESIAN_POINT('Ctrl Pts',(0.0388485409594955,0.322793218532066,
1.79357721819808));
#6528=CARTESIAN_POINT('Ctrl Pts',(-0.138202688744248,0.292642348031099,
1.80712928930927));
#6529=CARTESIAN_POINT('Ctrl Pts',(-0.271275014593156,0.173407667511399,
1.82061706508718));
#6530=CARTESIAN_POINT('Ctrl Pts',(-0.320408925286595,0.00250707464856787,
1.83403929175697));
#6531=CARTESIAN_POINT('Ctrl Pts',(-0.271307561449736,-0.167502591654885,
1.84739594116571));
#6532=CARTESIAN_POINT('Ctrl Pts',(-0.139930069519496,-0.284741206103476,
1.86068668924461));
#6533=CARTESIAN_POINT('Ctrl Pts',(0.0328273431379415,-0.313971999555478,
1.87391139490108));
#6534=CARTESIAN_POINT('Ctrl Pts',(0.193850817302591,-0.247125271575551,
1.88707004452662));
#6535=CARTESIAN_POINT('Ctrl Pts',(0.294125420947596,-0.105604428080939,
1.90016271438992));
#6536=CARTESIAN_POINT('Ctrl Pts',(0.303692393078913,0.0667945151618661,
1.91318971435693));
#6537=CARTESIAN_POINT('Ctrl Pts',(0.220491612017706,0.216911798478523,1.92615123879903));
#6538=CARTESIAN_POINT('Ctrl Pts',(0.0543221488869225,0.308989602518454,
1.94048115461963));
#6539=CARTESIAN_POINT('Ctrl Pts',(-0.157372149186157,0.277269028654297,
1.95615139456308));
#6540=CARTESIAN_POINT('Ctrl Pts',(-0.301541028549258,0.0952925261463745,
1.97313495002146));
#6541=CARTESIAN_POINT('Ctrl Pts',(-0.287140150837315,-0.0959909714068033,
1.98719573515425));
#6542=CARTESIAN_POINT('Ctrl Pts',(-0.200435907040306,-0.212440976387684,
1.99839033332071));
#6543=CARTESIAN_POINT('Ctrl Pts',(-0.0780453719389616,-0.28977073304184,
2.00955053962068));
#6544=CARTESIAN_POINT('Ctrl Pts',(0.0543569638846216,-0.289744106383568,
2.01926770009008));
#6545=CARTESIAN_POINT('Ctrl Pts',(0.149101826267907,-0.241622389761838,
2.0275666737348));
#6546=CARTESIAN_POINT('Ctrl Pts',(0.205114290476602,-0.198654311142817,
2.03309084965727));
#6547=CARTESIAN_POINT('Ctrl Pts',(0.27973233129585,-0.0981224791338798,
2.04273613227868));
#6548=CARTESIAN_POINT('Ctrl Pts',(0.294054838307538,0.0883885612962322,
2.05645362185213));
#6549=CARTESIAN_POINT('Ctrl Pts',(0.154021552042581,0.263442571251684,2.07282008366875));
#6550=CARTESIAN_POINT('Ctrl Pts',(-0.0473319417941907,0.293245461580669,
2.08774066257839));
#6551=CARTESIAN_POINT('Ctrl Pts',(-0.203892531954146,0.206287815842515,
2.10124325457571));
#6552=CARTESIAN_POINT('Ctrl Pts',(-0.281404389454363,0.0659836006472725,
2.11334963792451));
#6553=CARTESIAN_POINT('Ctrl Pts',(-0.2723714341636,-0.0936469583069963,
2.12541249039876));
#6554=CARTESIAN_POINT('Ctrl Pts',(-0.180144499604908,-0.22349377921263,
2.13743356131539));
#6555=CARTESIAN_POINT('Ctrl Pts',(-0.033449858406456,-0.284188291922273,
2.14941608862722));
#6556=CARTESIAN_POINT('Ctrl Pts',(0.122562408333805,-0.257670230647596,
2.16136028851425));
#6557=CARTESIAN_POINT('Ctrl Pts',(0.240186761064639,-0.15240311537952,2.17327325875895));
#6558=CARTESIAN_POINT('Ctrl Pts',(0.269167385254141,-0.0517780507002695,
2.18118730964103));
#6559=CARTESIAN_POINT('Ctrl Pts',(0.269174221747938,-0.00118166228325439,
2.18514810709965));
#6560=CARTESIAN_POINT('Ctrl Pts',(0.326819743817693,0.00167503652268494,
1.40864888399464));
#6561=CARTESIAN_POINT('Ctrl Pts',(0.326811467432193,0.0629279084542433,
1.41344389457114));
#6562=CARTESIAN_POINT('Ctrl Pts',(0.291654883267632,0.185084755965569,1.42305190526743));
#6563=CARTESIAN_POINT('Ctrl Pts',(0.148979195665167,0.312728390774808,1.43749916035482));
#6564=CARTESIAN_POINT('Ctrl Pts',(-0.0401862647160889,0.344885051828254,
1.45198374992715));
#6565=CARTESIAN_POINT('Ctrl Pts',(-0.217915663488207,0.271323343912871,
1.46650201744433));
#6566=CARTESIAN_POINT('Ctrl Pts',(-0.329503050990644,0.11413535024708,1.48105194869708));
#6567=CARTESIAN_POINT('Ctrl Pts',(-0.340379991513863,-0.0787520881849125,
1.49563081925542));
#6568=CARTESIAN_POINT('Ctrl Pts',(-0.270194290476258,-0.205738111213707,
1.50658459018308));
#6569=CARTESIAN_POINT('Ctrl Pts',(-0.199665121692685,-0.266881734670431,
1.51389467077294));
#6570=CARTESIAN_POINT('Ctrl Pts',(-0.160508386513694,-0.292302289608028,
1.51755114629707));
#6571=CARTESIAN_POINT('Ctrl Pts',(-0.118134791271926,-0.311933522239942,
1.52120901254844));
#6572=CARTESIAN_POINT('Ctrl Pts',(-0.00891167038672465,-0.34530394763833,
1.53015375485378));
#6573=CARTESIAN_POINT('Ctrl Pts',(0.183545882213297,-0.316669327909261,
1.54439993961451));
#6574=CARTESIAN_POINT('Ctrl Pts',(0.349995676828839,-0.107322625109419,
1.56396823487425));
#6575=CARTESIAN_POINT('Ctrl Pts',(0.331923882036601,0.137035034007625,1.58192781905788));
#6576=CARTESIAN_POINT('Ctrl Pts',(0.187023028957292,0.298335739363874,1.59826723674814));
#6577=CARTESIAN_POINT('Ctrl Pts',(-4.07900050576479E-5,0.352333628668086,
1.61297947284543));
#6578=CARTESIAN_POINT('Ctrl Pts',(-0.187515823756079,0.298337661946181,
1.62769561588367));
#6579=CARTESIAN_POINT('Ctrl Pts',(-0.317396577254554,0.152955414784301,
1.64241275153056));
#6580=CARTESIAN_POINT('Ctrl Pts',(-0.350074819871636,-0.0392507736732478,
1.65712799589898));
#6581=CARTESIAN_POINT('Ctrl Pts',(-0.275476950657307,-0.219299124116455,
1.67183845174987));
#6582=CARTESIAN_POINT('Ctrl Pts',(-0.116616564764591,-0.331999825553172,
1.68654123824752));
#6583=CARTESIAN_POINT('Ctrl Pts',(0.0777212807640258,-0.342885743881358,
1.70123348729869));
#6584=CARTESIAN_POINT('Ctrl Pts',(0.247890378833861,-0.248774962677378,
1.71591238391807));
#6585=CARTESIAN_POINT('Ctrl Pts',(0.341922241756374,-0.078821833086168,
1.73057458398919));
#6586=CARTESIAN_POINT('Ctrl Pts',(0.330944684888561,0.114920758632994,1.74521844664416));
#6587=CARTESIAN_POINT('Ctrl Pts',(0.218814809338252,0.272877094249764,1.75984029215667));
#6588=CARTESIAN_POINT('Ctrl Pts',(0.0401314023515666,0.346836885301389,
1.77443759960673));
#6589=CARTESIAN_POINT('Ctrl Pts',(-0.150221108850721,0.314496168181013,
1.78900816640339));
#6590=CARTESIAN_POINT('Ctrl Pts',(-0.293718171085479,0.18601886476932,1.80354799050301));
#6591=CARTESIAN_POINT('Ctrl Pts',(-0.346887342757174,0.00132400703486514,
1.81805626188758));
#6592=CARTESIAN_POINT('Ctrl Pts',(-0.29374715104042,-0.182902252872154,
1.83252961218796));
#6593=CARTESIAN_POINT('Ctrl Pts',(-0.151100609616018,-0.310278813236866,
1.84696571621268));
#6594=CARTESIAN_POINT('Ctrl Pts',(0.036937675316398,-0.342153332252125,
1.86136221026647));
#6595=CARTESIAN_POINT('Ctrl Pts',(0.212600699807242,-0.269287017513481,
1.8757168020348));
#6596=CARTESIAN_POINT('Ctrl Pts',(0.322231809337099,-0.114646253272976,
1.89002735257157));
#6597=CARTESIAN_POINT('Ctrl Pts',(0.332752609394029,0.0741069817676853,
1.9042916032421));
#6598=CARTESIAN_POINT('Ctrl Pts',(0.241542314658912,0.238754649423423,1.91850785152287));
#6599=CARTESIAN_POINT('Ctrl Pts',(0.0590639411267381,0.339919964670031,
1.93424736852057));
#6600=CARTESIAN_POINT('Ctrl Pts',(-0.17381495037296,0.305089861920068,1.95148870566044));
#6601=CARTESIAN_POINT('Ctrl Pts',(-0.332680466671874,0.104668687805014,
1.97019858165979));
#6602=CARTESIAN_POINT('Ctrl Pts',(-0.316831768055502,-0.10629215319313,
1.98570712860886));
#6603=CARTESIAN_POINT('Ctrl Pts',(-0.221152704671616,-0.234803595695131,
1.99806246070239));
#6604=CARTESIAN_POINT('Ctrl Pts',(-0.0860643901141648,-0.320165941287256,
2.01038082890037));
#6605=CARTESIAN_POINT('Ctrl Pts',(0.0601723380717702,-0.320146023962333,
2.02111670840766));
#6606=CARTESIAN_POINT('Ctrl Pts',(0.164800899338872,-0.26700416951472,2.03028161334532));
#6607=CARTESIAN_POINT('Ctrl Pts',(0.226657697996288,-0.21955265481665,2.03638255025733));
#6608=CARTESIAN_POINT('Ctrl Pts',(0.309065692640364,-0.108527426828177,
2.04703540530036));
#6609=CARTESIAN_POINT('Ctrl Pts',(0.324864915209835,0.0974261798297048,
2.0621845157232));
#6610=CARTESIAN_POINT('Ctrl Pts',(0.170289646488671,0.290611127431389,2.08025095052217));
#6611=CARTESIAN_POINT('Ctrl Pts',(-0.0517408616129622,0.323427973004647,
2.09670599777649));
#6612=CARTESIAN_POINT('Ctrl Pts',(-0.224161216243688,0.227626661550434,
2.11157970065908));
#6613=CARTESIAN_POINT('Ctrl Pts',(-0.309409326351099,0.0732552725630971,
2.1249004530645));
#6614=CARTESIAN_POINT('Ctrl Pts',(-0.299447065361936,-0.102125940306812,
2.13815531539376));
#6615=CARTESIAN_POINT('Ctrl Pts',(-0.198240680027746,-0.244539701723245,
2.15134406230612));
#6616=CARTESIAN_POINT('Ctrl Pts',(-0.037581548944414,-0.310964665237426,
2.16446709692427));
#6617=CARTESIAN_POINT('Ctrl Pts',(0.13292631747297,-0.281926222953237,2.17752364320475));
#6618=CARTESIAN_POINT('Ctrl Pts',(0.261173528224478,-0.167098336597803,
2.19051601295533));
#6619=CARTESIAN_POINT('Ctrl Pts',(0.292688581739866,-0.0575687444849278,
2.1991314360511));
#6620=CARTESIAN_POINT('Ctrl Pts',(0.292696006824134,-0.00261624123410937,
2.20343323983651));
#6621=CARTESIAN_POINT('Ctrl Pts',(0.308975662575307,0.00234251634852165,
1.40009150124657));
#6622=CARTESIAN_POINT('Ctrl Pts',(0.308967831215322,0.0603017897770032,
1.40462868163228));
#6623=CARTESIAN_POINT('Ctrl Pts',(0.27571613946542,0.17587293159813,1.41371870232149));
#6624=CARTESIAN_POINT('Ctrl Pts',(0.14052829168136,0.296880373272056,1.42741147339166));
#6625=CARTESIAN_POINT('Ctrl Pts',(-0.0390206409894663,0.327438852492569,
1.44115991935023));
#6626=CARTESIAN_POINT('Ctrl Pts',(-0.208015130690645,0.257544971295796,
1.45496360199322));
#6627=CARTESIAN_POINT('Ctrl Pts',(-0.31433121628426,0.107867391812847,1.46882103730561));
#6628=CARTESIAN_POINT('Ctrl Pts',(-0.324760930696744,-0.0761651731846545,
1.48273114655387));
#6629=CARTESIAN_POINT('Ctrl Pts',(-0.25770578826527,-0.197572131035348,
1.49320208134784));
#6630=CARTESIAN_POINT('Ctrl Pts',(-0.190205012752425,-0.256093277277717,
1.5001983760536));
#6631=CARTESIAN_POINT('Ctrl Pts',(-0.152711571444389,-0.280435204755278,
1.50369961169923));
#6632=CARTESIAN_POINT('Ctrl Pts',(-0.112116765219087,-0.299243448878827,
1.50720391497013));
#6633=CARTESIAN_POINT('Ctrl Pts',(-0.00742947447965367,-0.331230533315626,
1.51577743597841));
#6634=CARTESIAN_POINT('Ctrl Pts',(0.177344946592297,-0.303843669093901,
1.52945317895053));
#6635=CARTESIAN_POINT('Ctrl Pts',(0.337703669147259,-0.102384061208339,
1.54829190470144));
#6636=CARTESIAN_POINT('Ctrl Pts',(0.320386176990543,0.133556219760536,1.5656314880469));
#6637=CARTESIAN_POINT('Ctrl Pts',(0.180166649314842,0.289758997557382,1.58144797134203));
#6638=CARTESIAN_POINT('Ctrl Pts',(-0.00132206741687621,0.342212241169513,
1.59572221082199));
#6639=CARTESIAN_POINT('Ctrl Pts',(-0.183671702176775,0.289762637032663,
1.61003353536495));
#6640=CARTESIAN_POINT('Ctrl Pts',(-0.310342042497228,0.14807517418719,1.62437994961569));
#6641=CARTESIAN_POINT('Ctrl Pts',(-0.342344710230546,-0.0397483446680867,
1.63875921097831));
#6642=CARTESIAN_POINT('Ctrl Pts',(-0.26932802481127,-0.216162780784306,
1.65316909672021));
#6643=CARTESIAN_POINT('Ctrl Pts',(-0.11335028157701,-0.32690499085044,1.66760727054012));
#6644=CARTESIAN_POINT('Ctrl Pts',(0.0779896409308878,-0.337694308008293,
1.68207139079433));
#6645=CARTESIAN_POINT('Ctrl Pts',(0.245996504618211,-0.244859320987887,
1.69655892082441));
#6646=CARTESIAN_POINT('Ctrl Pts',(0.339122881244892,-0.0766951990321318,
1.71106887668148));
#6647=CARTESIAN_POINT('Ctrl Pts',(0.328303231554949,0.115536603234434,1.72559559277298));
#6648=CARTESIAN_POINT('Ctrl Pts',(0.216819416451737,0.272714660222625,1.74013907788606));
#6649=CARTESIAN_POINT('Ctrl Pts',(0.038629327840624,0.34654572302245,1.75469616476247));
#6650=CARTESIAN_POINT('Ctrl Pts',(-0.151730517540076,0.314282626901279,
1.76926319982864));
#6651=CARTESIAN_POINT('Ctrl Pts',(-0.295660631610015,0.185509220768529,
1.78384089368189));
#6652=CARTESIAN_POINT('Ctrl Pts',(-0.349181464322731,-0.000132902452383927,
1.79842245055717));
#6653=CARTESIAN_POINT('Ctrl Pts',(-0.295691618391146,-0.185833876958624,
1.81300730099236));
#6654=CARTESIAN_POINT('Ctrl Pts',(-0.151591431305487,-0.314604885214695,
1.82759256023074));
#6655=CARTESIAN_POINT('Ctrl Pts',(0.0389096325415752,-0.346969520413954,
1.84217561365937));
#6656=CARTESIAN_POINT('Ctrl Pts',(0.217372400747471,-0.273018514558698,
1.85675384492571));
#6657=CARTESIAN_POINT('Ctrl Pts',(0.329077169033808,-0.115573796608772,
1.87132449448901));
#6658=CARTESIAN_POINT('Ctrl Pts',(0.339888552571612,0.0771370427329227,
1.88588525710813));
#6659=CARTESIAN_POINT('Ctrl Pts',(0.246588824585348,0.245699401156214,1.90043285415478));
#6660=CARTESIAN_POINT('Ctrl Pts',(0.059383764715569,0.349570705626663,1.91658113980667));
#6661=CARTESIAN_POINT('Ctrl Pts',(-0.18025714962302,0.313891514320666,1.93431457393113));
#6662=CARTESIAN_POINT('Ctrl Pts',(-0.344390369949343,0.107068479425964,
1.95362750530272));
#6663=CARTESIAN_POINT('Ctrl Pts',(-0.328107849431858,-0.111399267400055,
1.96968435665062));
#6664=CARTESIAN_POINT('Ctrl Pts',(-0.228819035002148,-0.244801895274471,
1.98250464766913));
#6665=CARTESIAN_POINT('Ctrl Pts',(-0.0883888817388162,-0.333562219825158,
1.99531159404308));
#6666=CARTESIAN_POINT('Ctrl Pts',(0.06390108694825,-0.333615078896201,2.00648565100655));
#6667=CARTESIAN_POINT('Ctrl Pts',(0.17311235742343,-0.278151693895792,2.01605104836969));
#6668=CARTESIAN_POINT('Ctrl Pts',(0.237719738978489,-0.228592221119887,
2.0224225577694));
#6669=CARTESIAN_POINT('Ctrl Pts',(0.323887551888167,-0.112533970996369,
2.03355824516288));
#6670=CARTESIAN_POINT('Ctrl Pts',(0.340546892843711,0.103204150446501,2.04942473071775));
#6671=CARTESIAN_POINT('Ctrl Pts',(0.178299428106273,0.30616933398131,2.06839251648277));
#6672=CARTESIAN_POINT('Ctrl Pts',(-0.0554521422788362,0.340822969043152,
2.08571206561153));
#6673=CARTESIAN_POINT('Ctrl Pts',(-0.237391185083363,0.23979008338321,2.10140096499742));
#6674=CARTESIAN_POINT('Ctrl Pts',(-0.327514552494945,0.0766773806508595,
2.11547453862722));
#6675=CARTESIAN_POINT('Ctrl Pts',(-0.317013490278782,-0.108949377210494,
2.12950042186005));
#6676=CARTESIAN_POINT('Ctrl Pts',(-0.209773689761217,-0.259921362839895,
2.14347676014655));
#6677=CARTESIAN_POINT('Ctrl Pts',(-0.0392672842831704,-0.330457204877932,
2.15740251507558));
#6678=CARTESIAN_POINT('Ctrl Pts',(0.1419314616349,-0.299620592696538,2.17127537907273));
#6679=CARTESIAN_POINT('Ctrl Pts',(0.278394560994794,-0.177472560454167,
2.18509599978749));
#6680=CARTESIAN_POINT('Ctrl Pts',(0.311948936733415,-0.0607866435023563,
2.1942713847311));
#6681=CARTESIAN_POINT('Ctrl Pts',(0.311956844710082,-0.00226028906910728,
2.19885295751038));
#6682=CARTESIAN_POINT('Ctrl Pts',(0.299999683646987,0.00234130352927725,
1.40009150124657));
#6683=CARTESIAN_POINT('Ctrl Pts',(0.299992075807792,0.058646317336039,1.40449918252257));
#6684=CARTESIAN_POINT('Ctrl Pts',(0.267703823976176,0.170873854805974,1.41332597689034));
#6685=CARTESIAN_POINT('Ctrl Pts',(0.136388292868123,0.288427001435921,1.42662720914847));
#6686=CARTESIAN_POINT('Ctrl Pts',(-0.0380600582278086,0.318117946543192,
1.43998475699785));
#6687=CARTESIAN_POINT('Ctrl Pts',(-0.202303265104397,0.250195717548651,
1.45340015631867));
#6688=CARTESIAN_POINT('Ctrl Pts',(-0.305668184856449,0.104682534491432,
1.46687214536364));
#6689=CARTESIAN_POINT('Ctrl Pts',(-0.315820032591246,-0.0743007733969036,
1.48040059247731));
#6690=CARTESIAN_POINT('Ctrl Pts',(-0.250581817185145,-0.192431453073831,
1.49058865012208));
#6691=CARTESIAN_POINT('Ctrl Pts',(-0.184885616277594,-0.249388366415835,
1.49739790674125));
#6692=CARTESIAN_POINT('Ctrl Pts',(-0.148390241821198,-0.273082371347815,
1.50080595723938));
#6693=CARTESIAN_POINT('Ctrl Pts',(-0.108871032283292,-0.29139234917315,
1.50421741983629));
#6694=CARTESIAN_POINT('Ctrl Pts',(-0.0069453324122751,-0.322535646049005,
1.51256485573429));
#6695=CARTESIAN_POINT('Ctrl Pts',(0.173036139719135,-0.295879163364944,
1.52588654224678));
#6696=CARTESIAN_POINT('Ctrl Pts',(0.329381275573112,-0.0995231210697565,
1.54425036939462));
#6697=CARTESIAN_POINT('Ctrl Pts',(0.312519823715869,0.130664619012925,1.56116776183919));
#6698=CARTESIAN_POINT('Ctrl Pts',(0.175623409891217,0.283196568811908,1.57661184582646));
#6699=CARTESIAN_POINT('Ctrl Pts',(-0.00170640174969724,0.334465005486407,
1.59056005485894));
#6700=CARTESIAN_POINT('Ctrl Pts',(-0.180023541764348,0.283195393823563,
1.60455538622492));
#6701=CARTESIAN_POINT('Ctrl Pts',(-0.304003293840334,0.144546913461868,
1.61859632997908));
#6702=CARTESIAN_POINT('Ctrl Pts',(-0.335368767729676,-0.0394152680933303,
1.63268129545808));
#6703=CARTESIAN_POINT('Ctrl Pts',(-0.263809464751215,-0.212364713608931,
1.64680860320332));
#6704=CARTESIAN_POINT('Ctrl Pts',(-0.110777353802162,-0.321042679653587,
1.66097649136357));
#6705=CARTESIAN_POINT('Ctrl Pts',(0.0771377319574853,-0.331662145388596,
1.67518312328143));
#6706=CARTESIAN_POINT('Ctrl Pts',(0.242310499059917,-0.240422185372272,
1.68942658430208));
#6707=CARTESIAN_POINT('Ctrl Pts',(0.333965165875749,-0.0749639048060816,
1.70370489167579));
#6708=CARTESIAN_POINT('Ctrl Pts',(0.323334808639096,0.114391665751362,1.71801599173701));
#6709=CARTESIAN_POINT('Ctrl Pts',(0.213428807823085,0.269386973572793,1.73235777220482));
#6710=CARTESIAN_POINT('Ctrl Pts',(0.0375551957208218,0.342290293088701,
1.74672805867088));
#6711=CARTESIAN_POINT('Ctrl Pts',(-0.150552157108958,0.310435266995363,
1.76112462104241));
#6712=CARTESIAN_POINT('Ctrl Pts',(-0.292943546037226,0.183080826664645,
1.7755451807512));
#6713=CARTESIAN_POINT('Ctrl Pts',(-0.345971724616545,-0.000755050169826696,
1.78998741229651));
#6714=CARTESIAN_POINT('Ctrl Pts',(-0.292969625414991,-0.184869584225357,
1.80444894933381));
#6715=CARTESIAN_POINT('Ctrl Pts',(-0.149964130695888,-0.312702949838195,
1.81892738366057));
#6716=CARTESIAN_POINT('Ctrl Pts',(0.0393278383702601,-0.344893411306051,
1.83342028161105));
#6717=CARTESIAN_POINT('Ctrl Pts',(0.216880569645654,-0.271353329755712,
1.84792517694669));
#6718=CARTESIAN_POINT('Ctrl Pts',(0.32816306590606,-0.114557947655581,1.86243958044385));
#6719=CARTESIAN_POINT('Ctrl Pts',(0.338976565498085,0.077604733921516,1.87696098559129));
#6720=CARTESIAN_POINT('Ctrl Pts',(0.245857394029791,0.245901091257368,1.8914868739057));
#6721=CARTESIAN_POINT('Ctrl Pts',(0.0587650041824393,0.349754038023421,
1.90762891978624));
#6722=CARTESIAN_POINT('Ctrl Pts',(-0.181113967151586,0.314103429348402,
1.92538434383923));
#6723=CARTESIAN_POINT('Ctrl Pts',(-0.3457209249242,0.106820407791971,1.94474686926749));
#6724=CARTESIAN_POINT('Ctrl Pts',(-0.329429326627219,-0.112545408830404,
1.96087146849268));
#6725=CARTESIAN_POINT('Ctrl Pts',(-0.229624239431613,-0.246663510889421,
1.97376168226292));
#6726=CARTESIAN_POINT('Ctrl Pts',(-0.0883709022792632,-0.335964900532689,
1.98664460529397));
#6727=CARTESIAN_POINT('Ctrl Pts',(0.0650538569064664,-0.336061455964098,
1.99790631348129));
#6728=CARTESIAN_POINT('Ctrl Pts',(0.175154846512334,-0.280150232411291,
2.00754964965835));
#6729=CARTESIAN_POINT('Ctrl Pts',(0.240313024233827,-0.230169139256515,
2.01397587403001));
#6730=CARTESIAN_POINT('Ctrl Pts',(0.327278516892606,-0.113059531596934,
2.02521445394406));
#6731=CARTESIAN_POINT('Ctrl Pts',(0.344164783870684,0.104896799870906,2.04124691031968));
#6732=CARTESIAN_POINT('Ctrl Pts',(0.180057434020278,0.310325992459091,2.06044404323233));
#6733=CARTESIAN_POINT('Ctrl Pts',(-0.0568089689745267,0.345505318367412,
2.07799813231589));
#6734=CARTESIAN_POINT('Ctrl Pts',(-0.24141865243425,0.243028671458529,2.09391813720595));
#6735=CARTESIAN_POINT('Ctrl Pts',(-0.332978054716675,0.0773726024996246,
2.1082144881335));
#6736=CARTESIAN_POINT('Ctrl Pts',(-0.322327341410981,-0.111361257795146,
2.12247707319913));
#6737=CARTESIAN_POINT('Ctrl Pts',(-0.213201521733808,-0.265029708724835,
2.13670391728446));
#6738=CARTESIAN_POINT('Ctrl Pts',(-0.0395013579051905,-0.33691517309109,
2.15089294308459));
#6739=CARTESIAN_POINT('Ctrl Pts',(0.145288666887708,-0.305489063077451,
2.16504251556762));
#6740=CARTESIAN_POINT('Ctrl Pts',(0.284599775362727,-0.18083938172608,2.17915024381374));
#6741=CARTESIAN_POINT('Ctrl Pts',(0.318914082780001,-0.0616119635988021,
2.18852795857496));
#6742=CARTESIAN_POINT('Ctrl Pts',(0.318922161847072,-0.0018193816533177,
2.19320865445115));
#6743=CARTESIAN_POINT('',(0.299999683646987,0.00234130352927724,1.40009150124657));
#6744=CARTESIAN_POINT('Origin',(0.3,1.73141260914431E-17,1.43));
#6745=CARTESIAN_POINT('',(0.318922161847072,-0.00181938165331771,2.19320865445115));
#6746=CARTESIAN_POINT('Ctrl Pts',(0.299999683646987,0.00234130352927725,
1.40009150124657));
#6747=CARTESIAN_POINT('Ctrl Pts',(0.299992075807792,0.058646317336039,1.40449918252257));
#6748=CARTESIAN_POINT('Ctrl Pts',(0.267703823976176,0.170873854805974,1.41332597689034));
#6749=CARTESIAN_POINT('Ctrl Pts',(0.136388292868123,0.288427001435921,1.42662720914847));
#6750=CARTESIAN_POINT('Ctrl Pts',(-0.0380600582278086,0.318117946543192,
1.43998475699785));
#6751=CARTESIAN_POINT('Ctrl Pts',(-0.202303265104397,0.250195717548651,
1.45340015631867));
#6752=CARTESIAN_POINT('Ctrl Pts',(-0.305668184856449,0.104682534491432,
1.46687214536364));
#6753=CARTESIAN_POINT('Ctrl Pts',(-0.315820032591246,-0.0743007733969036,
1.48040059247731));
#6754=CARTESIAN_POINT('Ctrl Pts',(-0.250581817185145,-0.192431453073831,
1.49058865012208));
#6755=CARTESIAN_POINT('Ctrl Pts',(-0.184885616277594,-0.249388366415835,
1.49739790674125));
#6756=CARTESIAN_POINT('Ctrl Pts',(-0.148390241821198,-0.273082371347815,
1.50080595723938));
#6757=CARTESIAN_POINT('Ctrl Pts',(-0.108871032283292,-0.29139234917315,
1.50421741983629));
#6758=CARTESIAN_POINT('Ctrl Pts',(-0.0069453324122751,-0.322535646049005,
1.51256485573429));
#6759=CARTESIAN_POINT('Ctrl Pts',(0.173036139719135,-0.295879163364944,
1.52588654224678));
#6760=CARTESIAN_POINT('Ctrl Pts',(0.329381275573112,-0.0995231210697565,
1.54425036939462));
#6761=CARTESIAN_POINT('Ctrl Pts',(0.312519823715869,0.130664619012925,1.56116776183919));
#6762=CARTESIAN_POINT('Ctrl Pts',(0.175623409891217,0.283196568811908,1.57661184582646));
#6763=CARTESIAN_POINT('Ctrl Pts',(-0.00170640174969724,0.334465005486407,
1.59056005485894));
#6764=CARTESIAN_POINT('Ctrl Pts',(-0.180023541764348,0.283195393823563,
1.60455538622492));
#6765=CARTESIAN_POINT('Ctrl Pts',(-0.304003293840334,0.144546913461868,
1.61859632997908));
#6766=CARTESIAN_POINT('Ctrl Pts',(-0.335368767729676,-0.0394152680933303,
1.63268129545808));
#6767=CARTESIAN_POINT('Ctrl Pts',(-0.263809464751215,-0.212364713608931,
1.64680860320332));
#6768=CARTESIAN_POINT('Ctrl Pts',(-0.110777353802162,-0.321042679653587,
1.66097649136357));
#6769=CARTESIAN_POINT('Ctrl Pts',(0.0771377319574853,-0.331662145388596,
1.67518312328143));
#6770=CARTESIAN_POINT('Ctrl Pts',(0.242310499059917,-0.240422185372272,
1.68942658430208));
#6771=CARTESIAN_POINT('Ctrl Pts',(0.333965165875749,-0.0749639048060816,
1.70370489167579));
#6772=CARTESIAN_POINT('Ctrl Pts',(0.323334808639096,0.114391665751362,1.71801599173701));
#6773=CARTESIAN_POINT('Ctrl Pts',(0.213428807823085,0.269386973572793,1.73235777220482));
#6774=CARTESIAN_POINT('Ctrl Pts',(0.0375551957208218,0.342290293088701,
1.74672805867088));
#6775=CARTESIAN_POINT('Ctrl Pts',(-0.150552157108958,0.310435266995363,
1.76112462104241));
#6776=CARTESIAN_POINT('Ctrl Pts',(-0.292943546037226,0.183080826664645,
1.7755451807512));
#6777=CARTESIAN_POINT('Ctrl Pts',(-0.345971724616545,-0.000755050169826696,
1.78998741229651));
#6778=CARTESIAN_POINT('Ctrl Pts',(-0.292969625414991,-0.184869584225357,
1.80444894933381));
#6779=CARTESIAN_POINT('Ctrl Pts',(-0.149964130695888,-0.312702949838195,
1.81892738366057));
#6780=CARTESIAN_POINT('Ctrl Pts',(0.0393278383702601,-0.344893411306051,
1.83342028161105));
#6781=CARTESIAN_POINT('Ctrl Pts',(0.216880569645654,-0.271353329755712,
1.84792517694669));
#6782=CARTESIAN_POINT('Ctrl Pts',(0.32816306590606,-0.114557947655581,1.86243958044385));
#6783=CARTESIAN_POINT('Ctrl Pts',(0.338976565498085,0.077604733921516,1.87696098559129));
#6784=CARTESIAN_POINT('Ctrl Pts',(0.245857394029791,0.245901091257368,1.8914868739057));
#6785=CARTESIAN_POINT('Ctrl Pts',(0.0587650041824393,0.349754038023421,
1.90762891978624));
#6786=CARTESIAN_POINT('Ctrl Pts',(-0.181113967151586,0.314103429348402,
1.92538434383923));
#6787=CARTESIAN_POINT('Ctrl Pts',(-0.3457209249242,0.106820407791971,1.94474686926749));
#6788=CARTESIAN_POINT('Ctrl Pts',(-0.329429326627219,-0.112545408830404,
1.96087146849268));
#6789=CARTESIAN_POINT('Ctrl Pts',(-0.229624239431613,-0.246663510889421,
1.97376168226292));
#6790=CARTESIAN_POINT('Ctrl Pts',(-0.0883709022792632,-0.335964900532689,
1.98664460529397));
#6791=CARTESIAN_POINT('Ctrl Pts',(0.0650538569064664,-0.336061455964098,
1.99790631348129));
#6792=CARTESIAN_POINT('Ctrl Pts',(0.175154846512334,-0.280150232411291,
2.00754964965835));
#6793=CARTESIAN_POINT('Ctrl Pts',(0.240313024233827,-0.230169139256515,
2.01397587403001));
#6794=CARTESIAN_POINT('Ctrl Pts',(0.327278516892606,-0.113059531596934,
2.02521445394406));
#6795=CARTESIAN_POINT('Ctrl Pts',(0.344164783870684,0.104896799870906,2.04124691031968));
#6796=CARTESIAN_POINT('Ctrl Pts',(0.180057434020278,0.310325992459091,2.06044404323233));
#6797=CARTESIAN_POINT('Ctrl Pts',(-0.0568089689745267,0.345505318367412,
2.07799813231589));
#6798=CARTESIAN_POINT('Ctrl Pts',(-0.24141865243425,0.243028671458529,2.09391813720595));
#6799=CARTESIAN_POINT('Ctrl Pts',(-0.332978054716675,0.0773726024996246,
2.1082144881335));
#6800=CARTESIAN_POINT('Ctrl Pts',(-0.322327341410981,-0.111361257795146,
2.12247707319913));
#6801=CARTESIAN_POINT('Ctrl Pts',(-0.213201521733808,-0.265029708724835,
2.13670391728446));
#6802=CARTESIAN_POINT('Ctrl Pts',(-0.0395013579051905,-0.33691517309109,
2.15089294308459));
#6803=CARTESIAN_POINT('Ctrl Pts',(0.145288666887708,-0.305489063077451,
2.16504251556762));
#6804=CARTESIAN_POINT('Ctrl Pts',(0.284599775362727,-0.18083938172608,2.17915024381374));
#6805=CARTESIAN_POINT('Ctrl Pts',(0.318914082780001,-0.0616119635988021,
2.18852795857496));
#6806=CARTESIAN_POINT('Ctrl Pts',(0.318922161847072,-0.0018193816533177,
2.19320865445115));
#6807=CARTESIAN_POINT('Origin',(0.3,-3.60822483003176E-16,2.17));
#6808=CARTESIAN_POINT('Origin',(0.3,-3.60822483003176E-16,2.17));
#6809=CARTESIAN_POINT('Origin',(0.3,1.73141260914431E-17,1.43));
#6810=CARTESIAN_POINT('',(0.,0.,0.));
#6811=CARTESIAN_POINT('Origin',(0.,0.,4.8));
#6812=CARTESIAN_POINT('',(-0.16,-1.95943487863577E-17,5.));
#6813=CARTESIAN_POINT('Origin',(0.,0.,5.));
#6814=CARTESIAN_POINT('',(-0.16,-1.95943487863577E-17,4.8));
#6815=CARTESIAN_POINT('',(-0.16,-1.95943487863577E-17,4.8));
#6816=CARTESIAN_POINT('Origin',(0.,0.,4.8));
#6817=CARTESIAN_POINT('Origin',(0.,0.,4.8));
#6818=CARTESIAN_POINT('',(-2.2,-2.69422295812418E-16,5.));
#6819=CARTESIAN_POINT('Origin',(0.,0.,5.));
#6820=CARTESIAN_POINT('',(-2.2,-2.69422295812418E-16,4.8));
#6821=CARTESIAN_POINT('',(-2.2,-2.69422295812418E-16,4.8));
#6822=CARTESIAN_POINT('Origin',(0.,0.,4.8));
#6823=CARTESIAN_POINT('Origin',(0.,0.,5.));
#6824=CARTESIAN_POINT('Origin',(0.,0.,4.8));
#6825=CARTESIAN_POINT('',(0.,0.,0.));
#6826=CARTESIAN_POINT('Origin',(-6.2456986756515E-16,-3.4,4.9));
#6827=CARTESIAN_POINT('',(-0.275000000000001,-3.4,5.));
#6828=CARTESIAN_POINT('Origin',(-6.2456986756515E-16,-3.4,5.));
#6829=CARTESIAN_POINT('',(-0.275000000000001,-3.4,5.1));
#6830=CARTESIAN_POINT('',(-0.275000000000001,-3.4,4.9));
#6831=CARTESIAN_POINT('Origin',(-6.2456986756515E-16,-3.4,5.1));
#6832=CARTESIAN_POINT('Origin',(2.94448637286709,1.7,4.9));
#6833=CARTESIAN_POINT('',(2.66948637286709,1.7,5.));
#6834=CARTESIAN_POINT('Origin',(2.94448637286709,1.7,5.));
#6835=CARTESIAN_POINT('',(2.66948637286709,1.7,5.1));
#6836=CARTESIAN_POINT('',(2.66948637286709,1.7,4.9));
#6837=CARTESIAN_POINT('Origin',(2.94448637286709,1.7,5.1));
#6838=CARTESIAN_POINT('Origin',(2.0818995585505E-16,3.4,4.9));
#6839=CARTESIAN_POINT('',(-0.275,3.4,5.));
#6840=CARTESIAN_POINT('Origin',(2.0818995585505E-16,3.4,5.));
#6841=CARTESIAN_POINT('',(-0.275,3.4,5.1));
#6842=CARTESIAN_POINT('',(-0.275,3.4,4.9));
#6843=CARTESIAN_POINT('Origin',(2.0818995585505E-16,3.4,5.1));
#6844=CARTESIAN_POINT('Origin',(-2.94448637286709,1.7,4.9));
#6845=CARTESIAN_POINT('',(-3.21948637286709,1.7,5.));
#6846=CARTESIAN_POINT('Origin',(-2.94448637286709,1.7,5.));
#6847=CARTESIAN_POINT('',(-3.21948637286709,1.7,5.1));
#6848=CARTESIAN_POINT('',(-3.21948637286709,1.7,4.9));
#6849=CARTESIAN_POINT('Origin',(-2.94448637286709,1.7,5.1));
#6850=CARTESIAN_POINT('Origin',(-2.94448637286709,-1.7,4.9));
#6851=CARTESIAN_POINT('',(-3.21948637286709,-1.7,5.));
#6852=CARTESIAN_POINT('Origin',(-2.94448637286709,-1.7,5.));
#6853=CARTESIAN_POINT('',(-3.21948637286709,-1.7,5.1));
#6854=CARTESIAN_POINT('',(-3.21948637286709,-1.7,4.9));
#6855=CARTESIAN_POINT('Origin',(-2.94448637286709,-1.7,5.1));
#6856=CARTESIAN_POINT('Origin',(2.94448637286709,-1.7,4.9));
#6857=CARTESIAN_POINT('',(2.66948637286709,-1.7,5.));
#6858=CARTESIAN_POINT('Origin',(2.94448637286709,-1.7,5.));
#6859=CARTESIAN_POINT('',(2.66948637286709,-1.7,5.1));
#6860=CARTESIAN_POINT('',(2.66948637286709,-1.7,4.9));
#6861=CARTESIAN_POINT('Origin',(2.94448637286709,-1.7,5.1));
#6862=CARTESIAN_POINT('Origin',(0.,0.,5.));
#6863=CARTESIAN_POINT('',(-0.16,-1.95943487863577E-17,5.1));
#6864=CARTESIAN_POINT('Origin',(0.,0.,5.1));
#6865=CARTESIAN_POINT('',(-0.16,-1.95943487863577E-17,5.));
#6866=CARTESIAN_POINT('',(-0.16,-1.95943487863577E-17,5.));
#6867=CARTESIAN_POINT('Origin',(0.,0.,5.));
#6868=CARTESIAN_POINT('Origin',(0.,0.,5.));
#6869=CARTESIAN_POINT('',(-4.,-4.89858719658941E-16,5.1));
#6870=CARTESIAN_POINT('Origin',(0.,0.,5.1));
#6871=CARTESIAN_POINT('',(-4.,-4.89858719658941E-16,5.));
#6872=CARTESIAN_POINT('',(-4.,-4.89858719658941E-16,5.));
#6873=CARTESIAN_POINT('Origin',(0.,0.,5.));
#6874=CARTESIAN_POINT('Origin',(0.,0.,5.1));
#6875=CARTESIAN_POINT('Origin',(0.,0.,5.));
#6876=CARTESIAN_POINT('',(0.,0.,0.));
#6877=CARTESIAN_POINT('Origin',(0.,0.,5.3));
#6878=CARTESIAN_POINT('',(-0.41,-5.02105187650415E-17,5.7));
#6879=CARTESIAN_POINT('Origin',(0.,0.,5.7));
#6880=CARTESIAN_POINT('',(-0.41,-5.02105187650415E-17,5.3));
#6881=CARTESIAN_POINT('',(-0.41,-5.02105187650415E-17,5.3));
#6882=CARTESIAN_POINT('Origin',(0.,0.,5.3));
#6883=CARTESIAN_POINT('Origin',(0.,0.,5.3));
#6884=CARTESIAN_POINT('',(-0.6,-7.34788079488412E-17,5.7));
#6885=CARTESIAN_POINT('Origin',(0.,0.,5.7));
#6886=CARTESIAN_POINT('',(-0.6,-7.34788079488412E-17,5.3));
#6887=CARTESIAN_POINT('',(-0.6,-7.34788079488412E-17,5.3));
#6888=CARTESIAN_POINT('Origin',(0.,0.,5.3));
#6889=CARTESIAN_POINT('Origin',(0.,0.,5.7));
#6890=CARTESIAN_POINT('Origin',(0.,0.,5.3));
#6891=CARTESIAN_POINT('',(-2.2,-2.69422295812418E-16,5.3));
#6892=CARTESIAN_POINT('Origin',(0.,0.,5.3));
#6893=CARTESIAN_POINT('Origin',(0.,0.,5.1));
#6894=CARTESIAN_POINT('',(-0.16,-1.95943487863577E-17,5.3));
#6895=CARTESIAN_POINT('Origin',(0.,0.,5.3));
#6896=CARTESIAN_POINT('',(-0.16,-1.95943487863577E-17,5.1));
#6897=CARTESIAN_POINT('',(-0.16,-1.95943487863577E-17,5.1));
#6898=CARTESIAN_POINT('Origin',(0.,0.,5.1));
#6899=CARTESIAN_POINT('Origin',(0.,0.,5.1));
#6900=CARTESIAN_POINT('',(-2.2,-2.69422295812418E-16,5.1));
#6901=CARTESIAN_POINT('',(-2.2,-2.69422295812418E-16,5.1));
#6902=CARTESIAN_POINT('Origin',(0.,0.,5.1));
#6903=CARTESIAN_POINT('Origin',(0.,0.,5.3));
#6904=CARTESIAN_POINT('Origin',(0.,0.,5.1));
#6905=CARTESIAN_POINT('',(0.,0.,0.));
#6906=CARTESIAN_POINT('Origin',(-6.66133814775094E-16,-3.4,6.5));
#6907=CARTESIAN_POINT('',(-0.318956006072959,-2.98299632352941,6.5));
#6908=CARTESIAN_POINT('',(0.318956006072958,-2.98299632352941,6.5));
#6909=CARTESIAN_POINT('Origin',(0.,0.,6.5));
#6910=CARTESIAN_POINT('Origin',(-6.2456986756515E-16,-3.4,6.5));
#6911=CARTESIAN_POINT('Origin',(-6.2456986756515E-16,-3.4,5.7));
#6912=CARTESIAN_POINT('',(-0.318956006072959,-2.98299632352941,5.7));
#6913=CARTESIAN_POINT('',(-0.318956006072959,-2.98299632352941,5.7));
#6914=CARTESIAN_POINT('',(0.318956006072958,-2.98299632352941,5.7));
#6915=CARTESIAN_POINT('Origin',(-6.2456986756515E-16,-3.4,5.7));
#6916=CARTESIAN_POINT('',(0.318956006072958,-2.98299632352941,5.7));
#6917=CARTESIAN_POINT('Origin',(2.94448637286709,1.7,5.7));
#6918=CARTESIAN_POINT('',(2.42387259253558,1.76772216571351,6.5));
#6919=CARTESIAN_POINT('',(2.42387259253558,1.76772216571351,5.7));
#6920=CARTESIAN_POINT('',(2.42387259253558,1.76772216571351,5.7));
#6921=CARTESIAN_POINT('',(2.74282859860853,1.2152741578159,6.5));
#6922=CARTESIAN_POINT('Origin',(2.94448637286709,1.7,6.5));
#6923=CARTESIAN_POINT('',(2.74282859860853,1.2152741578159,5.7));
#6924=CARTESIAN_POINT('',(2.74282859860853,1.2152741578159,5.7));
#6925=CARTESIAN_POINT('Origin',(2.94448637286709,1.7,5.7));
#6926=CARTESIAN_POINT('Origin',(2.94448637286709,1.7,6.5));
#6927=CARTESIAN_POINT('Origin',(0.,0.,6.5));
#6928=CARTESIAN_POINT('Origin',(2.22044604925031E-16,3.4,6.5));
#6929=CARTESIAN_POINT('',(0.318956006072958,2.98299632352941,6.5));
#6930=CARTESIAN_POINT('',(-0.318956006072958,2.98299632352941,6.5));
#6931=CARTESIAN_POINT('Origin',(0.,0.,6.5));
#6932=CARTESIAN_POINT('Origin',(2.0818995585505E-16,3.4,6.5));
#6933=CARTESIAN_POINT('Origin',(2.0818995585505E-16,3.4,5.7));
#6934=CARTESIAN_POINT('',(0.318956006072958,2.98299632352941,5.7));
#6935=CARTESIAN_POINT('',(0.318956006072958,2.98299632352941,5.7));
#6936=CARTESIAN_POINT('',(-0.318956006072958,2.98299632352941,5.7));
#6937=CARTESIAN_POINT('Origin',(2.0818995585505E-16,3.4,5.7));
#6938=CARTESIAN_POINT('',(-0.318956006072958,2.98299632352941,5.7));
#6939=CARTESIAN_POINT('Origin',(-2.94448637286709,1.7,6.5));
#6940=CARTESIAN_POINT('',(-2.42387259253558,1.76772216571351,6.5));
#6941=CARTESIAN_POINT('',(-2.74282859860853,1.2152741578159,6.5));
#6942=CARTESIAN_POINT('Origin',(0.,0.,6.5));
#6943=CARTESIAN_POINT('Origin',(-2.94448637286709,1.7,6.5));
#6944=CARTESIAN_POINT('Origin',(-2.94448637286709,1.7,5.7));
#6945=CARTESIAN_POINT('',(-2.42387259253558,1.76772216571351,5.7));
#6946=CARTESIAN_POINT('',(-2.42387259253558,1.76772216571351,5.7));
#6947=CARTESIAN_POINT('',(-2.74282859860853,1.2152741578159,5.7));
#6948=CARTESIAN_POINT('Origin',(-2.94448637286709,1.7,5.7));
#6949=CARTESIAN_POINT('',(-2.74282859860853,1.2152741578159,5.7));
#6950=CARTESIAN_POINT('Origin',(-2.94448637286709,-1.7,6.5));
#6951=CARTESIAN_POINT('',(-2.74282859860853,-1.2152741578159,6.5));
#6952=CARTESIAN_POINT('',(-2.42387259253558,-1.76772216571351,6.5));
#6953=CARTESIAN_POINT('Origin',(0.,0.,6.5));
#6954=CARTESIAN_POINT('Origin',(-2.94448637286709,-1.7,6.5));
#6955=CARTESIAN_POINT('Origin',(-2.94448637286709,-1.7,5.7));
#6956=CARTESIAN_POINT('',(-2.74282859860853,-1.2152741578159,5.7));
#6957=CARTESIAN_POINT('',(-2.74282859860853,-1.2152741578159,5.7));
#6958=CARTESIAN_POINT('',(-2.42387259253558,-1.76772216571351,5.7));
#6959=CARTESIAN_POINT('Origin',(-2.94448637286709,-1.7,5.7));
#6960=CARTESIAN_POINT('',(-2.42387259253558,-1.76772216571351,5.7));
#6961=CARTESIAN_POINT('Origin',(2.94448637286709,-1.7,5.7));
#6962=CARTESIAN_POINT('',(2.74282859860853,-1.2152741578159,6.5));
#6963=CARTESIAN_POINT('',(2.74282859860853,-1.2152741578159,5.7));
#6964=CARTESIAN_POINT('',(2.74282859860853,-1.2152741578159,5.7));
#6965=CARTESIAN_POINT('',(2.42387259253558,-1.76772216571351,6.5));
#6966=CARTESIAN_POINT('Origin',(2.94448637286709,-1.7,6.5));
#6967=CARTESIAN_POINT('',(2.42387259253558,-1.76772216571351,5.7));
#6968=CARTESIAN_POINT('',(2.42387259253558,-1.76772216571351,5.7));
#6969=CARTESIAN_POINT('Origin',(2.94448637286709,-1.7,5.7));
#6970=CARTESIAN_POINT('Origin',(2.94448637286709,-1.7,6.5));
#6971=CARTESIAN_POINT('Origin',(0.,0.,6.5));
#6972=CARTESIAN_POINT('Origin',(0.,0.,5.7));
#6973=CARTESIAN_POINT('',(-3.,-3.67394039744206E-16,9.5));
#6974=CARTESIAN_POINT('Origin',(0.,0.,9.5));
#6975=CARTESIAN_POINT('',(-3.,-3.67394039744206E-16,5.7));
#6976=CARTESIAN_POINT('',(-3.,-3.67394039744206E-16,5.7));
#6977=CARTESIAN_POINT('Origin',(0.,0.,5.7));
#6978=CARTESIAN_POINT('Origin',(0.,0.,5.7));
#6979=CARTESIAN_POINT('Origin',(0.,0.,5.7));
#6980=CARTESIAN_POINT('Origin',(0.,0.,5.7));
#6981=CARTESIAN_POINT('Origin',(0.,0.,5.7));
#6982=CARTESIAN_POINT('Origin',(0.,0.,5.7));
#6983=CARTESIAN_POINT('Origin',(0.,0.,5.7));
#6984=CARTESIAN_POINT('Origin',(-6.2456986756515E-16,-3.4,4.9));
#6985=CARTESIAN_POINT('',(-0.275000000000001,-3.4,5.1));
#6986=CARTESIAN_POINT('Origin',(-6.2456986756515E-16,-3.4,5.1));
#6987=CARTESIAN_POINT('',(-0.275000000000001,-3.4,5.7));
#6988=CARTESIAN_POINT('',(-0.275000000000001,-3.4,4.9));
#6989=CARTESIAN_POINT('Origin',(-6.2456986756515E-16,-3.4,5.7));
#6990=CARTESIAN_POINT('Origin',(2.94448637286709,1.7,4.9));
#6991=CARTESIAN_POINT('',(2.66948637286709,1.7,5.1));
#6992=CARTESIAN_POINT('Origin',(2.94448637286709,1.7,5.1));
#6993=CARTESIAN_POINT('',(2.66948637286709,1.7,5.7));
#6994=CARTESIAN_POINT('',(2.66948637286709,1.7,4.9));
#6995=CARTESIAN_POINT('Origin',(2.94448637286709,1.7,5.7));
#6996=CARTESIAN_POINT('Origin',(2.0818995585505E-16,3.4,4.9));
#6997=CARTESIAN_POINT('',(-0.275,3.4,5.1));
#6998=CARTESIAN_POINT('Origin',(2.0818995585505E-16,3.4,5.1));
#6999=CARTESIAN_POINT('',(-0.275,3.4,5.7));
#7000=CARTESIAN_POINT('',(-0.275,3.4,4.9));
#7001=CARTESIAN_POINT('Origin',(2.0818995585505E-16,3.4,5.7));
#7002=CARTESIAN_POINT('Origin',(-2.94448637286709,1.7,4.9));
#7003=CARTESIAN_POINT('',(-3.21948637286709,1.7,5.1));
#7004=CARTESIAN_POINT('Origin',(-2.94448637286709,1.7,5.1));
#7005=CARTESIAN_POINT('',(-3.21948637286709,1.7,5.7));
#7006=CARTESIAN_POINT('',(-3.21948637286709,1.7,4.9));
#7007=CARTESIAN_POINT('Origin',(-2.94448637286709,1.7,5.7));
#7008=CARTESIAN_POINT('Origin',(-2.94448637286709,-1.7,4.9));
#7009=CARTESIAN_POINT('',(-3.21948637286709,-1.7,5.1));
#7010=CARTESIAN_POINT('Origin',(-2.94448637286709,-1.7,5.1));
#7011=CARTESIAN_POINT('',(-3.21948637286709,-1.7,5.7));
#7012=CARTESIAN_POINT('',(-3.21948637286709,-1.7,4.9));
#7013=CARTESIAN_POINT('Origin',(-2.94448637286709,-1.7,5.7));
#7014=CARTESIAN_POINT('Origin',(2.94448637286709,-1.7,4.9));
#7015=CARTESIAN_POINT('',(2.66948637286709,-1.7,5.1));
#7016=CARTESIAN_POINT('Origin',(2.94448637286709,-1.7,5.1));
#7017=CARTESIAN_POINT('',(2.66948637286709,-1.7,5.7));
#7018=CARTESIAN_POINT('',(2.66948637286709,-1.7,4.9));
#7019=CARTESIAN_POINT('Origin',(2.94448637286709,-1.7,5.7));
#7020=CARTESIAN_POINT('Origin',(0.,0.,8.7));
#7021=CARTESIAN_POINT('',(-0.34,-4.163799117101E-17,8.8));
#7022=CARTESIAN_POINT('Origin',(0.,0.,8.8));
#7023=CARTESIAN_POINT('',(-0.34,4.163799117101E-17,9.5));
#7024=CARTESIAN_POINT('',(-0.34,-4.163799117101E-17,8.7));
#7025=CARTESIAN_POINT('Origin',(0.,0.,9.5));
#7026=CARTESIAN_POINT('Origin',(0.,0.,5.));
#7027=CARTESIAN_POINT('',(-2.5,-3.06161699786838E-16,5.1));
#7028=CARTESIAN_POINT('Origin',(0.,0.,5.1));
#7029=CARTESIAN_POINT('',(-2.5,-3.06161699786838E-16,8.8));
#7030=CARTESIAN_POINT('',(-2.5,-3.06161699786838E-16,5.));
#7031=CARTESIAN_POINT('Origin',(0.,0.,8.8));
#7032=CARTESIAN_POINT('Origin',(0.,0.,8.8));
#7033=CARTESIAN_POINT('Origin',(0.,0.,9.5));
#7034=CARTESIAN_POINT('Origin',(0.,0.,5.1));
#7035=CARTESIAN_POINT('',(-4.,-4.89858719658941E-16,5.7));
#7036=CARTESIAN_POINT('Origin',(0.,0.,5.7));
#7037=CARTESIAN_POINT('',(-4.,-4.89858719658941E-16,5.1));
#7038=CARTESIAN_POINT('',(-4.,-4.89858719658941E-16,5.1));
#7039=CARTESIAN_POINT('Origin',(0.,0.,5.1));
#7040=CARTESIAN_POINT('Origin',(0.,0.,5.7));
#7041=CARTESIAN_POINT('Origin',(0.,0.,5.1));
#7042=CARTESIAN_POINT('',(0.,0.,0.));
#7043=CARTESIAN_POINT('Ctrl Pts',(0.799999065628721,0.00692558823944229,
5.30024010712383));
#7044=CARTESIAN_POINT('Ctrl Pts',(0.799974755250737,0.187114846749742,5.31274930893178));
#7045=CARTESIAN_POINT('Ctrl Pts',(0.674578200671659,0.546127076651831,5.33781512365923));
#7046=CARTESIAN_POINT('Ctrl Pts',(0.187998995393781,0.852903359039399,5.37564381521248));
#7047=CARTESIAN_POINT('Ctrl Pts',(-0.386721866921525,0.788448388841122,
5.41368605209984));
#7048=CARTESIAN_POINT('Ctrl Pts',(-0.7983994419892,0.377627224111744,5.45194644400096));
#7049=CARTESIAN_POINT('Ctrl Pts',(-0.864375113399524,-0.203617876612744,
5.49042055747836));
#7050=CARTESIAN_POINT('Ctrl Pts',(-0.552019639313923,-0.701812288635587,
5.52910737914477));
#7051=CARTESIAN_POINT('Ctrl Pts',(0.00615426428515267,-0.897757418326962,
5.56800374230524));
#7052=CARTESIAN_POINT('Ctrl Pts',(0.463089276607972,-0.737891299975203,
5.59986549204054));
#7053=CARTESIAN_POINT('Ctrl Pts',(0.706662565433678,-0.474149107376678,
5.62457829573124));
#7054=CARTESIAN_POINT('Ctrl Pts',(0.854347338563578,-0.169471123140589,
5.6478904398873));
#7055=CARTESIAN_POINT('Ctrl Pts',(0.854381411403854,0.269671075667267,5.67712918390586));
#7056=CARTESIAN_POINT('Ctrl Pts',(0.581578462406747,0.670744438556907,5.70943359497258));
#7057=CARTESIAN_POINT('Ctrl Pts',(0.189982000930166,0.858805851522918,5.73891161848027));
#7058=CARTESIAN_POINT('Ctrl Pts',(-0.201854620920769,0.859148371452269,
5.76552549972421));
#7059=CARTESIAN_POINT('Ctrl Pts',(-0.556170302204947,0.688486751453872,
5.79222147180784));
#7060=CARTESIAN_POINT('Ctrl Pts',(-0.802120584542054,0.380288702719923,
5.81899788702529));
#7061=CARTESIAN_POINT('Ctrl Pts',(-0.890321102734134,-0.0053444036833259,
5.84585301727138));
#7062=CARTESIAN_POINT('Ctrl Pts',(-0.816781798992104,-0.327577127496462,
5.86829638740099));
#7063=CARTESIAN_POINT('Ctrl Pts',(-0.678277859648778,-0.547664335405585,
5.88628859994389));
#7064=CARTESIAN_POINT('Ctrl Pts',(-0.494316135451619,-0.731945478665225,
5.90430550175064));
#7065=CARTESIAN_POINT('Ctrl Pts',(-0.194941007989142,-0.876310026230692,
5.92687230420244));
#7066=CARTESIAN_POINT('Ctrl Pts',(0.204945568353256,-0.876409485122255,
5.95402353339188));
#7067=CARTESIAN_POINT('Ctrl Pts',(0.566325487118899,-0.702556101088839,
5.98124373289334));
#7068=CARTESIAN_POINT('Ctrl Pts',(0.816751045229916,-0.388463305588866,
6.00853075028047));
#7069=CARTESIAN_POINT('Ctrl Pts',(0.917174982875959,0.0480250206861584,
6.03892142694837));
#7070=CARTESIAN_POINT('Ctrl Pts',(0.768829350780382,0.528866010776267,6.07244001895545));
#7071=CARTESIAN_POINT('Ctrl Pts',(0.338627495917749,0.872873034891815,6.10911095186911));
#7072=CARTESIAN_POINT('Ctrl Pts',(-0.212178222814091,0.914151313349766,
6.14588130840082));
#7073=CARTESIAN_POINT('Ctrl Pts',(-0.691759933067223,0.637451614256161,
6.18274515756461));
#7074=CARTESIAN_POINT('Ctrl Pts',(-0.932934482256533,0.137697594997002,
6.21969639210087));
#7075=CARTESIAN_POINT('Ctrl Pts',(-0.84730393945114,-0.435496308403701,
6.25827178793966));
#7076=CARTESIAN_POINT('Ctrl Pts',(-0.415273257958933,-0.868240176171726,
6.29847623644814));
#7077=CARTESIAN_POINT('Ctrl Pts',(0.146189896678077,-0.930950222024402,
6.33566388079779));
#7078=CARTESIAN_POINT('Ctrl Pts',(0.578787425776111,-0.722091726547751,
6.36825221458814));
#7079=CARTESIAN_POINT('Ctrl Pts',(0.835229259505866,-0.400278931762148,
6.3962159259868));
#7080=CARTESIAN_POINT('Ctrl Pts',(0.943177486850013,0.0688606453452641,
6.42887288667825));
#7081=CARTESIAN_POINT('Ctrl Pts',(0.756462512495389,0.604750444420971,6.46623690685835));
#7082=CARTESIAN_POINT('Ctrl Pts',(0.214509054547464,0.945343920852135,6.50831791566041));
#7083=CARTESIAN_POINT('Ctrl Pts',(-0.421585054233784,0.873670673138226,
6.55043539297339));
#7084=CARTESIAN_POINT('Ctrl Pts',(-0.874725713994987,0.420703846750279,
6.59257924943873));
#7085=CARTESIAN_POINT('Ctrl Pts',(-0.946491736933492,-0.216206220818672,
6.63473932973225));
#7086=CARTESIAN_POINT('Ctrl Pts',(-0.605472064685913,-0.758979181442101,
6.67690544450194));
#7087=CARTESIAN_POINT('Ctrl Pts',(-0.000509641250504898,-0.970641038681315,
6.71906739492544));
#7088=CARTESIAN_POINT('Ctrl Pts',(0.604236817182525,-0.758999928674301,
6.76121498571335));
#7089=CARTESIAN_POINT('Ctrl Pts',(0.944676427167983,-0.216670516455945,
6.80333805746961));
#7090=CARTESIAN_POINT('Ctrl Pts',(0.873719648783539,0.418956634979468,6.8454265042638));
#7091=CARTESIAN_POINT('Ctrl Pts',(0.421037273012308,0.871132652579719,6.88747029453994));
#7092=CARTESIAN_POINT('Ctrl Pts',(-0.142342851291253,0.933831870869633,
6.92479402146672));
#7093=CARTESIAN_POINT('Ctrl Pts',(-0.575104466317865,0.724476767443434,
6.95741054274359));
#7094=CARTESIAN_POINT('Ctrl Pts',(-0.831597121038275,0.403171008458228,
6.98533606563364));
#7095=CARTESIAN_POINT('Ctrl Pts',(-0.922808904665035,0.00254068286457492,
7.01322724854536));
#7096=CARTESIAN_POINT('Ctrl Pts',(-0.831484359832733,-0.397369041930912,
7.04108128388358));
#7097=CARTESIAN_POINT('Ctrl Pts',(-0.576024516479058,-0.717622866946566,
7.06889539860548));
#7098=CARTESIAN_POINT('Ctrl Pts',(-0.207464718971416,-0.895095126308869,
7.09666685370961));
#7099=CARTESIAN_POINT('Ctrl Pts',(0.200869050822812,-0.894893573965507,
7.12439296344474));
#7100=CARTESIAN_POINT('Ctrl Pts',(0.568135301656786,-0.717941543510051,
7.15207107099507));
#7101=CARTESIAN_POINT('Ctrl Pts',(0.821742493579341,-0.399813712939291,
7.17969857736332));
#7102=CARTESIAN_POINT('Ctrl Pts',(0.912100647381109,-0.00372699171446918,
7.20727292857109));
#7103=CARTESIAN_POINT('Ctrl Pts',(0.821667160899362,0.391120281113409,7.23479162069698));
#7104=CARTESIAN_POINT('Ctrl Pts',(0.527798142032111,0.760706416566583,7.26682897888736));
#7105=CARTESIAN_POINT('Ctrl Pts',(0.00437094025093319,0.944184514671381,
7.30334225024583));
#7106=CARTESIAN_POINT('Ctrl Pts',(-0.583164611559206,0.738086874931468,
7.3442757526392));
#7107=CARTESIAN_POINT('Ctrl Pts',(-0.912546668924433,0.213026529714121,
7.38505770065783));
#7108=CARTESIAN_POINT('Ctrl Pts',(-0.843060529623956,-0.400706652853849,
7.42568118182012));
#7109=CARTESIAN_POINT('Ctrl Pts',(-0.407835437985135,-0.835237258109269,
7.46613873367218));
#7110=CARTESIAN_POINT('Ctrl Pts',(0.200737244244076,-0.903598468057941,
7.5064251969444));
#7111=CARTESIAN_POINT('Ctrl Pts',(0.71672352100227,-0.578479045751934,7.54653146106904));
#7112=CARTESIAN_POINT('Ctrl Pts',(0.849917343436364,-0.197265324952655,
7.57314919120958));
#7113=CARTESIAN_POINT('Ctrl Pts',(0.849943147209423,-0.00600671278230411,
7.58642685605973));
#7114=CARTESIAN_POINT('Ctrl Pts',(0.770079135866838,0.00692155156817904,
5.30024010712383));
#7115=CARTESIAN_POINT('Ctrl Pts',(0.770055720112496,0.180479832525886,5.31228896941391));
#7116=CARTESIAN_POINT('Ctrl Pts',(0.649347137055222,0.526118956744516,5.33641790275693));
#7117=CARTESIAN_POINT('Ctrl Pts',(0.180677599950648,0.821679099419469,5.37285586761231));
#7118=CARTESIAN_POINT('Ctrl Pts',(-0.373128354027995,0.759596327571503,
5.40950951731212));
#7119=CARTESIAN_POINT('Ctrl Pts',(-0.770051450984494,0.363580245990391,
5.44639246645647));
#7120=CARTESIAN_POINT('Ctrl Pts',(-0.833750732775199,-0.197081341774288,
5.48350071817735));
#7121=CARTESIAN_POINT('Ctrl Pts',(-0.532331315046715,-0.677969641751496,
5.5208364575171));
#7122=CARTESIAN_POINT('Ctrl Pts',(0.00675318837749655,-0.867294541965757,
5.558400781988));
#7123=CARTESIAN_POINT('Ctrl Pts',(0.448424688054875,-0.712845112569316,
5.58919119813692));
#7124=CARTESIAN_POINT('Ctrl Pts',(0.684012778929899,-0.457765801730765,
5.61309167265538));
#7125=CARTESIAN_POINT('Ctrl Pts',(0.82691455168644,-0.162993811747473,5.6356443242608));
#7126=CARTESIAN_POINT('Ctrl Pts',(0.82699649983482,0.262124971545771,5.66394696022895));
#7127=CARTESIAN_POINT('Ctrl Pts',(0.562750276158912,0.650752034831193,5.69524212629919));
#7128=CARTESIAN_POINT('Ctrl Pts',(0.183080725565527,0.833119661747386,5.72381920452852));
#7129=CARTESIAN_POINT('Ctrl Pts',(-0.197084703463694,0.833490239824234,
5.74963623066415));
#7130=CARTESIAN_POINT('Ctrl Pts',(-0.541119975074503,0.667809968168665,
5.77555492059187));
#7131=CARTESIAN_POINT('Ctrl Pts',(-0.780113947482257,0.368392103745768,
5.80156649252668));
#7132=CARTESIAN_POINT('Ctrl Pts',(-0.865905134963049,-0.00656170868815412,
5.82767483842523));
#7133=CARTESIAN_POINT('Ctrl Pts',(-0.794375852743549,-0.320111204417347,
5.84950881094256));
#7134=CARTESIAN_POINT('Ctrl Pts',(-0.659521269028743,-0.534410811061921,
5.86702622272765));
#7135=CARTESIAN_POINT('Ctrl Pts',(-0.480335340635082,-0.713917263728105,
5.88457460840773));
#7136=CARTESIAN_POINT('Ctrl Pts',(-0.188587087034294,-0.854642083096481,
5.90656315000717));
#7137=CARTESIAN_POINT('Ctrl Pts',(0.201462529249485,-0.854779640403169,
5.9330427097564));
#7138=CARTESIAN_POINT('Ctrl Pts',(0.554262072476138,-0.685098200004362,
5.95961046024728));
#7139=CARTESIAN_POINT('Ctrl Pts',(0.798967352085236,-0.378235706832728,
5.98626742358202));
#7140=CARTESIAN_POINT('Ctrl Pts',(0.89721847916451,0.0485845903033819,6.01597993297972));
#7141=CARTESIAN_POINT('Ctrl Pts',(0.752070839701578,0.519313731169816,6.04878757680353));
#7142=CARTESIAN_POINT('Ctrl Pts',(0.330497979661169,0.856564661134425,6.08472490306161));
#7143=CARTESIAN_POINT('Ctrl Pts',(-0.209973066601811,0.897165035883339,
6.12079612560753));
#7144=CARTESIAN_POINT('Ctrl Pts',(-0.68120970786282,0.625397209779933,6.15700765884533));
#7145=CARTESIAN_POINT('Ctrl Pts',(-0.918572438612158,0.13378828614086,6.19335554838198));
#7146=CARTESIAN_POINT('Ctrl Pts',(-0.83433799028855,-0.430850802296383,
6.23134861625561));
#7147=CARTESIAN_POINT('Ctrl Pts',(-0.408316865658928,-0.857793214073537,
6.2709938323838));
#7148=CARTESIAN_POINT('Ctrl Pts',(0.146288162282126,-0.919868958459814,
6.30771962173879));
#7149=CARTESIAN_POINT('Ctrl Pts',(0.574223288772557,-0.71333190916663,6.33995134748923));
#7150=CARTESIAN_POINT('Ctrl Pts',(0.828161465810104,-0.394717048019018,
6.36763553346922));
#7151=CARTESIAN_POINT('Ctrl Pts',(0.935214831817973,0.0702367246280078,
6.39999872706231));
#7152=CARTESIAN_POINT('Ctrl Pts',(0.750063250540666,0.602049612066996,6.43706602732403));
#7153=CARTESIAN_POINT('Ctrl Pts',(0.211520380136952,0.940697836629915,6.47888152979277));
#7154=CARTESIAN_POINT('Ctrl Pts',(-0.421676436247289,0.869510362169926,
6.52079671898647));
#7155=CARTESIAN_POINT('Ctrl Pts',(-0.873553921061096,0.418039168812721,
6.56280406058959));
#7156=CARTESIAN_POINT('Ctrl Pts',(-0.945379508760524,-0.217899113421901,
6.60489250808515));
#7157=CARTESIAN_POINT('Ctrl Pts',(-0.604485708962148,-0.760787236561161,
6.64705240063428));
#7158=CARTESIAN_POINT('Ctrl Pts',(0.00138176225817566,-0.972945250150102,
6.6892731978663));
#7159=CARTESIAN_POINT('Ctrl Pts',(0.608080140735397,-0.760798630125154,
6.73154461863783));
#7160=CARTESIAN_POINT('Ctrl Pts',(0.950239792824421,-0.216025881173973,
6.77385551750453));
#7161=CARTESIAN_POINT('Ctrl Pts',(0.879017289772042,0.423590907490335,6.81620268596198));
#7162=CARTESIAN_POINT('Ctrl Pts',(0.422960901581898,0.879362908068112,6.85856017311708));
#7163=CARTESIAN_POINT('Ctrl Pts',(-0.145593093231334,0.942790559668914,
6.89621968364161));
#7164=CARTESIAN_POINT('Ctrl Pts',(-0.582932490358213,0.73127758858104,6.92917512678282));
#7165=CARTESIAN_POINT('Ctrl Pts',(-0.842401988544835,0.406320842666593,
6.957415448388));
#7166=CARTESIAN_POINT('Ctrl Pts',(-0.934795701286156,0.000685604828614038,
6.985653769321));
#7167=CARTESIAN_POINT('Ctrl Pts',(-0.842294766840471,-0.404603381671274,
7.01387715318084));
#7168=CARTESIAN_POINT('Ctrl Pts',(-0.583187447906784,-0.729494778082508,
7.04208836805485));
#7169=CARTESIAN_POINT('Ctrl Pts',(-0.20899792340701,-0.909726737101999,
7.07028057033796));
#7170=CARTESIAN_POINT('Ctrl Pts',(0.206012719667752,-0.909558569724805,
7.09845804612497));
#7171=CARTESIAN_POINT('Ctrl Pts',(0.579624839727756,-0.72959465407811,7.12660922044297));
#7172=CARTESIAN_POINT('Ctrl Pts',(0.837867106227739,-0.405711083857505,
7.15473493621397));
#7173=CARTESIAN_POINT('Ctrl Pts',(0.929983985732294,-0.00207542308664412,
7.18283200361311));
#7174=CARTESIAN_POINT('Ctrl Pts',(0.837775922394786,0.40066931879227,7.21089711007051));
#7175=CARTESIAN_POINT('Ctrl Pts',(0.537807840870324,0.777996358577212,7.24360025784798));
#7176=CARTESIAN_POINT('Ctrl Pts',(0.00294143852372089,0.965597941956312,
7.28090792189502));
#7177=CARTESIAN_POINT('Ctrl Pts',(-0.59827790503141,0.754837569025208,7.32278668150169));
#7178=CARTESIAN_POINT('Ctrl Pts',(-0.935814946990508,0.217001877726337,
7.36456027598379));
#7179=CARTESIAN_POINT('Ctrl Pts',(-0.864667175323564,-0.412475523451113,
7.40622093849563));
#7180=CARTESIAN_POINT('Ctrl Pts',(-0.417866766747618,-0.858729006758795,
7.44775776125507));
#7181=CARTESIAN_POINT('Ctrl Pts',(0.207655975088153,-0.929085997388315,
7.48916462895728));
#7182=CARTESIAN_POINT('Ctrl Pts',(0.73862266392267,-0.594662305466805,7.53042707168622));
#7183=CARTESIAN_POINT('Ctrl Pts',(0.875837799539084,-0.201989676969171,
7.55784229424685));
#7184=CARTESIAN_POINT('Ctrl Pts',(0.875864379853922,-0.00497530564290791,
7.5715195387037));
#7185=CARTESIAN_POINT('Ctrl Pts',(0.710428941733949,0.00492953088558486,
5.32881831830437));
#7186=CARTESIAN_POINT('Ctrl Pts',(0.71040731614315,0.165219065394011,5.33994603008611));
#7187=CARTESIAN_POINT('Ctrl Pts',(0.599024128589712,0.483870366740507,5.3621924509196));
#7188=CARTESIAN_POINT('Ctrl Pts',(0.167205166996449,0.75612127364975,5.39576440291455));
#7189=CARTESIAN_POINT('Ctrl Pts',(-0.342469011252512,0.698867316238289,
5.42949607339388));
#7190=CARTESIAN_POINT('Ctrl Pts',(-0.707447256311363,0.334638873927445,
5.46341601587375));
#7191=CARTESIAN_POINT('Ctrl Pts',(-0.765942731942805,-0.180685845273631,
5.49752276624412));
#7192=CARTESIAN_POINT('Ctrl Pts',(-0.488977975671522,-0.622493468082251,
5.53182729600019));
#7193=CARTESIAN_POINT('Ctrl Pts',(0.00623870066985125,-0.79639957834953,
5.56633555615365));
#7194=CARTESIAN_POINT('Ctrl Pts',(0.411979748797062,-0.65451285296037,5.59462344155862));
#7195=CARTESIAN_POINT('Ctrl Pts',(0.628431910779513,-0.420156210117234,
5.61658281146561));
#7196=CARTESIAN_POINT('Ctrl Pts',(0.759739764112401,-0.149292484888909,
5.63730747934422));
#7197=CARTESIAN_POINT('Ctrl Pts',(0.759837930575591,0.241447639232068,5.66332246132793));
#7198=CARTESIAN_POINT('Ctrl Pts',(0.516864570620339,0.598828714990839,5.6921027083035));
#7199=CARTESIAN_POINT('Ctrl Pts',(0.16754402090728,0.766642660816134,5.7183984452765));
#7200=CARTESIAN_POINT('Ctrl Pts',(-0.18243289406626,0.766996703299491,5.74216819224318));
#7201=CARTESIAN_POINT('Ctrl Pts',(-0.499344694617947,0.614409373974203,
5.7660436717059));
#7202=CARTESIAN_POINT('Ctrl Pts',(-0.719666388043044,0.338417073722969,
5.79002421526266));
#7203=CARTESIAN_POINT('Ctrl Pts',(-0.798838486989696,-0.00747184320142611,
5.81411179267834));
#7204=CARTESIAN_POINT('Ctrl Pts',(-0.732821087254027,-0.296979929993814,
5.83427424859502));
#7205=CARTESIAN_POINT('Ctrl Pts',(-0.608236501384017,-0.494969333219339,
5.85045910955365));
#7206=CARTESIAN_POINT('Ctrl Pts',(-0.442617486739659,-0.660891288693568,
5.8666802534398));
#7207=CARTESIAN_POINT('Ctrl Pts',(-0.172748327050428,-0.791093551297648,
5.88702427548063));
#7208=CARTESIAN_POINT('Ctrl Pts',(0.188434824933959,-0.791259517626132,
5.91154722254856));
#7209=CARTESIAN_POINT('Ctrl Pts',(0.515509148139609,-0.63399975107043,5.93618028019028));
#7210=CARTESIAN_POINT('Ctrl Pts',(0.742660619778638,-0.349226128508519,
5.96092404661359));
#7211=CARTESIAN_POINT('Ctrl Pts',(0.834013573979388,0.047387173011833,5.98854018010049));
#7212=CARTESIAN_POINT('Ctrl Pts',(0.699054298781812,0.485509196729349,6.01907630606175));
#7213=CARTESIAN_POINT('Ctrl Pts',(0.306089489608805,0.800037047528466,6.05258598067156));
#7214=CARTESIAN_POINT('Ctrl Pts',(-0.198806257075136,0.83811783046203,6.08629244673437));
#7215=CARTESIAN_POINT('Ctrl Pts',(-0.639994604888811,0.58386009688861,6.12019546148202));
#7216=CARTESIAN_POINT('Ctrl Pts',(-0.862778510831916,0.122809110352501,
6.15429381358228));
#7217=CARTESIAN_POINT('Ctrl Pts',(-0.783768475044449,-0.408002461396071,
6.19001514975991));
#7218=CARTESIAN_POINT('Ctrl Pts',(-0.382461984654271,-0.810530499122485,
6.22738726758261));
#7219=CARTESIAN_POINT('Ctrl Pts',(0.141571880318707,-0.869426431241229,
6.26209856247513));
#7220=CARTESIAN_POINT('Ctrl Pts',(0.546857792365987,-0.673923824775829,
6.29262411862805));
#7221=CARTESIAN_POINT('Ctrl Pts',(0.787850231799947,-0.371686474029746,
6.31889326617887));
#7222=CARTESIAN_POINT('Ctrl Pts',(0.889701212277186,0.0702541647771362,
6.34966096595927));
#7223=CARTESIAN_POINT('Ctrl Pts',(0.713512875154728,0.577124702757749,6.38499463961466));
#7224=CARTESIAN_POINT('Ctrl Pts',(0.198967909509621,0.901053551471294,6.42496855240101));
#7225=CARTESIAN_POINT('Ctrl Pts',(-0.408089575093021,0.833131022176632,
6.46516128973043));
#7226=CARTESIAN_POINT('Ctrl Pts',(-0.842862380754781,0.399211540997894,
6.50556671739343));
#7227=CARTESIAN_POINT('Ctrl Pts',(-0.912482057616401,-0.214227019813974,
6.54617863195434));
#7228=CARTESIAN_POINT('Ctrl Pts',(-0.582857572239619,-0.739804921207224,
6.58699019870486));
#7229=CARTESIAN_POINT('Ctrl Pts',(0.00529210032697009,-0.946120388887076,
6.62799422182894));
#7230=CARTESIAN_POINT('Ctrl Pts',(0.596417413889089,-0.73978975515068,6.66918308377763));
#7231=CARTESIAN_POINT('Ctrl Pts',(0.931157121946736,-0.20751322428765,6.71054882574604));
#7232=CARTESIAN_POINT('Ctrl Pts',(0.861650483779265,0.419727599707763,6.75208097200662));
#7233=CARTESIAN_POINT('Ctrl Pts',(0.413147604956643,0.868498049400113,6.79377525221771));
#7234=CARTESIAN_POINT('Ctrl Pts',(-0.148210983168275,0.931421962876526,
6.83097036528324));
#7235=CARTESIAN_POINT('Ctrl Pts',(-0.581294729795694,0.722118347875597,
6.86360544825447));
#7236=CARTESIAN_POINT('Ctrl Pts',(-0.838871906802363,0.399682199015836,
6.89163933377065));
#7237=CARTESIAN_POINT('Ctrl Pts',(-0.930877231252504,-0.00373870819751691,
6.91972773631357));
#7238=CARTESIAN_POINT('Ctrl Pts',(-0.838749751075799,-0.407817095097561,
6.94787183402895));
#7239=CARTESIAN_POINT('Ctrl Pts',(-0.579931993725618,-0.732521582072749,
6.9760659349542));
#7240=CARTESIAN_POINT('Ctrl Pts',(-0.205212822112969,-0.913124822787424,
7.00430873475179));
#7241=CARTESIAN_POINT('Ctrl Pts',(0.211338054228992,-0.913070414334495,
7.03259350527625));
#7242=CARTESIAN_POINT('Ctrl Pts',(0.587263134138024,-0.732110657981568,
7.06092123472863));
#7243=CARTESIAN_POINT('Ctrl Pts',(0.847742099102453,-0.405599817717801,
7.08928670598057));
#7244=CARTESIAN_POINT('Ctrl Pts',(0.940948978785284,0.00228770078596691,
7.1176867396323));
#7245=CARTESIAN_POINT('Ctrl Pts',(0.847659354457111,0.410238520315532,7.14611819660086));
#7246=CARTESIAN_POINT('Ctrl Pts',(0.543275903219406,0.793339172582683,7.17932027275837));
#7247=CARTESIAN_POINT('Ctrl Pts',(-0.001093578869141,0.984623315384901,
7.21730924712761));
#7248=CARTESIAN_POINT('Ctrl Pts',(-0.615252284949225,0.769726133995085,
7.26008973650359));
#7249=CARTESIAN_POINT('Ctrl Pts',(-0.961422256849412,0.218820343216691,
7.30290266259028));
#7250=CARTESIAN_POINT('Ctrl Pts',(-0.888633848724617,-0.428292780832149,
7.34573759998394));
#7251=CARTESIAN_POINT('Ctrl Pts',(-0.42811642962634,-0.888746898872104,
7.38857936211361));
#7252=CARTESIAN_POINT('Ctrl Pts',(0.218959376739582,-0.961833511797225,
7.43142516328682));
#7253=CARTESIAN_POINT('Ctrl Pts',(0.770122900311167,-0.615157339727794,
7.47424382285298));
#7254=CARTESIAN_POINT('Ctrl Pts',(0.913207865694905,-0.206388594750497,
7.5027957331042));
#7255=CARTESIAN_POINT('Ctrl Pts',(0.913235549072487,-0.00119827763899913,
7.51704057274925));
#7256=CARTESIAN_POINT('Ctrl Pts',(0.688502394196997,-0.00177585944161231,
5.42536374837757));
#7257=CARTESIAN_POINT('Ctrl Pts',(0.688481448875166,0.153471500858794,5.43614141945633));
#7258=CARTESIAN_POINT('Ctrl Pts',(0.580508040541705,0.46124670025465,5.45764245524231));
#7259=CARTESIAN_POINT('Ctrl Pts',(0.165662319023174,0.722161337503787,5.48987538957648));
#7260=CARTESIAN_POINT('Ctrl Pts',(-0.320578571387279,0.667050889553626,
5.52206618528612));
#7261=CARTESIAN_POINT('Ctrl Pts',(-0.666378826232044,0.32127882597957,5.55424091986707));
#7262=CARTESIAN_POINT('Ctrl Pts',(-0.721063694800031,-0.164642450695304,
5.58640440743116));
#7263=CARTESIAN_POINT('Ctrl Pts',(-0.461013415699651,-0.578597703078686,
5.61857188153771));
#7264=CARTESIAN_POINT('Ctrl Pts',(0.000868763121645957,-0.740322038056404,
5.65075229330461));
#7265=CARTESIAN_POINT('Ctrl Pts',(0.377087016267437,-0.608394442936668,
5.67699673395361));
#7266=CARTESIAN_POINT('Ctrl Pts',(0.577057627822796,-0.391810817241549,
5.69729012722977));
#7267=CARTESIAN_POINT('Ctrl Pts',(0.698092236754842,-0.142020837867168,
5.71640197572506));
#7268=CARTESIAN_POINT('Ctrl Pts',(0.697963439505406,0.21710900600399,5.74031529151263));
#7269=CARTESIAN_POINT('Ctrl Pts',(0.475355133020151,0.544099194249106,5.76666169992576));
#7270=CARTESIAN_POINT('Ctrl Pts',(0.156654851678278,0.697080460332168,5.79065302227195));
#7271=CARTESIAN_POINT('Ctrl Pts',(-0.161711917448867,0.697304453295988,
5.81227877536069));
#7272=CARTESIAN_POINT('Ctrl Pts',(-0.449161842092396,0.558802207686871,
5.83393922469739));
#7273=CARTESIAN_POINT('Ctrl Pts',(-0.648454473279016,0.309008113535057,
5.85564132087709));
#7274=CARTESIAN_POINT('Ctrl Pts',(-0.719837707005216,-0.00322310267600228,
5.8773860839056));
#7275=CARTESIAN_POINT('Ctrl Pts',(-0.660324209075774,-0.263926195140504,
5.89554604949557));
#7276=CARTESIAN_POINT('Ctrl Pts',(-0.548312630732919,-0.441913047209008,
5.91009721234879));
#7277=CARTESIAN_POINT('Ctrl Pts',(-0.399568209162923,-0.590912445741052,
5.92466534563453));
#7278=CARTESIAN_POINT('Ctrl Pts',(-0.157550820881924,-0.70761172499092,
5.94291010238594));
#7279=CARTESIAN_POINT('Ctrl Pts',(0.165683821816319,-0.707692893763189,
5.96485832442363));
#7280=CARTESIAN_POINT('Ctrl Pts',(0.457834734757014,-0.567156151977817,
5.98686542599537));
#7281=CARTESIAN_POINT('Ctrl Pts',(0.660365135739603,-0.313163685177989,
6.00893343132688));
#7282=CARTESIAN_POINT('Ctrl Pts',(0.741647053339758,0.0400023925443897,
6.03352542353788));
#7283=CARTESIAN_POINT('Ctrl Pts',(0.6215856897095,0.429424608756888,6.0606712019436));
#7284=CARTESIAN_POINT('Ctrl Pts',(0.272788863259715,0.708464025234,6.09040985442785));
#7285=CARTESIAN_POINT('Ctrl Pts',(-0.174640201386968,0.742128787355836,
6.12028246378202));
#7286=CARTESIAN_POINT('Ctrl Pts',(-0.565102038705666,0.517026489502915,
6.1502917775661));
#7287=CARTESIAN_POINT('Ctrl Pts',(-0.762043624567604,0.109327312662896,
6.18044350600909));
#7288=CARTESIAN_POINT('Ctrl Pts',(-0.692189456122551,-0.359678326088431,
6.21200701480215));
#7289=CARTESIAN_POINT('Ctrl Pts',(-0.337773460931687,-0.715129603852559,
6.24501197076816));
#7290=CARTESIAN_POINT('Ctrl Pts',(0.124866016940657,-0.767119798247897,
6.27565761479799));
#7291=CARTESIAN_POINT('Ctrl Pts',(0.482663833907203,-0.594530247737682,
6.30260654020584));
#7292=CARTESIAN_POINT('Ctrl Pts',(0.695450511759543,-0.32768100442103,6.32580056862507));
#7293=CARTESIAN_POINT('Ctrl Pts',(0.785412896461935,0.0626075158038052,
6.35297268106789));
#7294=CARTESIAN_POINT('Ctrl Pts',(0.629799785153589,0.510459438093438,6.38419099540486));
#7295=CARTESIAN_POINT('Ctrl Pts',(0.174872432500897,0.796962684150136,6.41953687685404));
#7296=CARTESIAN_POINT('Ctrl Pts',(-0.362484676752387,0.736952725256016,
6.4551134881321));
#7297=CARTESIAN_POINT('Ctrl Pts',(-0.74792746534711,0.35245915978463,6.49092474388711));
#7298=CARTESIAN_POINT('Ctrl Pts',(-0.809887309570728,-0.192065947901566,
6.52697449126839));
#7299=CARTESIAN_POINT('Ctrl Pts',(-0.516915158076634,-0.65954619222211,
6.56326583721123));
#7300=CARTESIAN_POINT('Ctrl Pts',(0.00709632936792426,-0.843579839117015,
6.59980147205316));
#7301=CARTESIAN_POINT('Ctrl Pts',(0.535080054211952,-0.659528972736876,
6.63658345012356));
#7302=CARTESIAN_POINT('Ctrl Pts',(0.834961098454938,-0.183143056575008,
6.67361341976074));
#7303=CARTESIAN_POINT('Ctrl Pts',(0.772836475154942,0.379911298835229,6.71089252375131));
#7304=CARTESIAN_POINT('Ctrl Pts',(0.369319867823668,0.784090370590367,6.74842072124706));
#7305=CARTESIAN_POINT('Ctrl Pts',(-0.137507651352654,0.841177037621035,
6.78200064499767));
#7306=CARTESIAN_POINT('Ctrl Pts',(-0.529655686323561,0.651783755111279,
6.81154496618753));
#7307=CARTESIAN_POINT('Ctrl Pts',(-0.763440172149879,0.359289385813127,
6.83697845361481));
#7308=CARTESIAN_POINT('Ctrl Pts',(-0.847211586055085,-0.0075813723717918,
6.86252259094478));
#7309=CARTESIAN_POINT('Ctrl Pts',(-0.763337400290734,-0.37595112739322,
6.88817526440515));
#7310=CARTESIAN_POINT('Ctrl Pts',(-0.526914388323573,-0.672730225787424,
6.91393691075106));
#7311=CARTESIAN_POINT('Ctrl Pts',(-0.183698562689997,-0.838276618909781,
6.93980597887144));
#7312=CARTESIAN_POINT('Ctrl Pts',(0.198889088741007,-0.838335964394735,
6.96578323697683));
#7313=CARTESIAN_POINT('Ctrl Pts',(0.545106947003364,-0.67180754918665,6.99186582148597));
#7314=CARTESIAN_POINT('Ctrl Pts',(0.785703595073577,-0.370406649743822,
7.01805361583897));
#7315=CARTESIAN_POINT('Ctrl Pts',(0.872119316826772,0.00721196141493378,
7.04434542939925));
#7316=CARTESIAN_POINT('Ctrl Pts',(0.785618184490446,0.386004597261683,7.07073989965295));
#7317=CARTESIAN_POINT('Ctrl Pts',(0.502331801959327,0.742799085163601,7.10165209474801));
#7318=CARTESIAN_POINT('Ctrl Pts',(-0.00621863503242753,0.921910367253639,
7.13714527690347));
#7319=CARTESIAN_POINT('Ctrl Pts',(-0.582851103775203,0.720649175322028,
7.17729562502998));
#7320=CARTESIAN_POINT('Ctrl Pts',(-0.909668842554882,0.201440782148561,
7.21765904401918));
#7321=CARTESIAN_POINT('Ctrl Pts',(-0.841213659251149,-0.41162272843365,
7.25823121418976));
#7322=CARTESIAN_POINT('Ctrl Pts',(-0.403262459624705,-0.850227454077078,
7.29900198947476));
#7323=CARTESIAN_POINT('Ctrl Pts',(0.215483513378321,-0.920627886099326,
7.33997190269741));
#7324=CARTESIAN_POINT('Ctrl Pts',(0.745429336505933,-0.587899220267355,
7.3811170115228));
#7325=CARTESIAN_POINT('Ctrl Pts',(0.883871797949062,-0.193227595737394,
7.40868621059601));
#7326=CARTESIAN_POINT('Ctrl Pts',(0.8838985919702,0.0053707753556189,7.42247342039135));
#7327=CARTESIAN_POINT('Ctrl Pts',(0.750293052325257,-0.00715957249020984,
5.50303372536175));
#7328=CARTESIAN_POINT('Ctrl Pts',(0.750270265731315,0.161735352510056,5.51475884548619));
#7329=CARTESIAN_POINT('Ctrl Pts',(0.632695708259348,0.496355890433882,5.53813632129441));
#7330=CARTESIAN_POINT('Ctrl Pts',(0.18381648383294,0.778081359279531,5.57298649818651));
#7331=CARTESIAN_POINT('Ctrl Pts',(-0.339280552431234,0.718378415257623,
5.6076202896276));
#7332=CARTESIAN_POINT('Ctrl Pts',(-0.709001801655557,0.347985187059841,
5.64204689091912));
#7333=CARTESIAN_POINT('Ctrl Pts',(-0.766698885918436,-0.16919180614749,
5.67627188750895));
#7334=CARTESIAN_POINT('Ctrl Pts',(-0.491102255096102,-0.606944769908898,
5.71030250431352));
#7335=CARTESIAN_POINT('Ctrl Pts',(-0.00508600093609879,-0.776552326514125,
5.74414714312887));
#7336=CARTESIAN_POINT('Ctrl Pts',(0.388081485630343,-0.638236893263609,
5.77157703947433));
#7337=CARTESIAN_POINT('Ctrl Pts',(0.596158844376195,-0.412773207290159,
5.79269814069561));
#7338=CARTESIAN_POINT('Ctrl Pts',(0.721744080724043,-0.15346691557969,5.81253217830301));
#7339=CARTESIAN_POINT('Ctrl Pts',(0.721291797138653,0.217701679185308,5.83724463136508));
#7340=CARTESIAN_POINT('Ctrl Pts',(0.492248297398938,0.553560023202817,5.86431639993153));
#7341=CARTESIAN_POINT('Ctrl Pts',(0.166319730891556,0.709798906698298,5.88884215604732));
#7342=CARTESIAN_POINT('Ctrl Pts',(-0.157783238149665,0.709878237357754,
5.9108529793775));
#7343=CARTESIAN_POINT('Ctrl Pts',(-0.449076273551193,0.569337590676698,
5.9328067996584));
#7344=CARTESIAN_POINT('Ctrl Pts',(-0.650064161571041,0.317172677340155,
5.95470251296732));
#7345=CARTESIAN_POINT('Ctrl Pts',(-0.721621885005776,0.00344024431033504,
5.97654562679051));
#7346=CARTESIAN_POINT('Ctrl Pts',(-0.661964542748072,-0.257286466758943,
5.99470556888389));
#7347=CARTESIAN_POINT('Ctrl Pts',(-0.550269179200512,-0.434720760832016,
6.00921182085571));
#7348=CARTESIAN_POINT('Ctrl Pts',(-0.402276742496014,-0.58292974874922,
6.02370295744568));
#7349=CARTESIAN_POINT('Ctrl Pts',(-0.162278225783224,-0.698511519651894,
6.04178723904388));
#7350=CARTESIAN_POINT('Ctrl Pts',(0.15678598762643,-0.698434753182134,6.06344900909546));
#7351=CARTESIAN_POINT('Ctrl Pts',(0.443832361536606,-0.560174670954122,
6.0850728430943));
#7352=CARTESIAN_POINT('Ctrl Pts',(0.641886657484862,-0.311548705127534,
6.10666325451466));
#7353=CARTESIAN_POINT('Ctrl Pts',(0.720903708581916,0.0325797868375459,
6.13061738623125));
#7354=CARTESIAN_POINT('Ctrl Pts',(0.604189885592221,0.409985700434759,6.15692940855218));
#7355=CARTESIAN_POINT('Ctrl Pts',(0.267732283871283,0.678698793729311,6.1855932204343));
#7356=CARTESIAN_POINT('Ctrl Pts',(-0.161176377088454,0.710602415331958,
6.2142207026778));
#7357=CARTESIAN_POINT('Ctrl Pts',(-0.53324499976805,0.49569736156826,6.2428252689349));
#7358=CARTESIAN_POINT('Ctrl Pts',(-0.71970802918005,0.108916638193807,6.27141553040571));
#7359=CARTESIAN_POINT('Ctrl Pts',(-0.653459538269235,-0.333490314335375,
6.30118792123758));
#7360=CARTESIAN_POINT('Ctrl Pts',(-0.320608653043408,-0.666665722932101,
6.33214798295712));
#7361=CARTESIAN_POINT('Ctrl Pts',(0.11110066391128,-0.714779997862643,6.36073732994674));
#7362=CARTESIAN_POINT('Ctrl Pts',(0.443426222920022,-0.554309028733026,
6.38577168766062));
#7363=CARTESIAN_POINT('Ctrl Pts',(0.640332263629123,-0.307185736963075,
6.4072429033775));
#7364=CARTESIAN_POINT('Ctrl Pts',(0.723203970884255,0.0529817392810816,
6.43231277693535));
#7365=CARTESIAN_POINT('Ctrl Pts',(0.579875213873492,0.464421357446747,6.46099511352603));
#7366=CARTESIAN_POINT('Ctrl Pts',(0.163540281833546,0.726164737539782,6.49332268601409));
#7367=CARTESIAN_POINT('Ctrl Pts',(-0.325806422280217,0.671154653749907,
6.52571901232898));
#7368=CARTESIAN_POINT('Ctrl Pts',(-0.675167952131389,0.322177709778464,
6.55819617950246));
#7369=CARTESIAN_POINT('Ctrl Pts',(-0.730838200739421,-0.169856078141101,
6.59076464701581));
#7370=CARTESIAN_POINT('Ctrl Pts',(-0.466820433339978,-0.590588090246883,
6.62343536526493));
#7371=CARTESIAN_POINT('Ctrl Pts',(0.00350996735505748,-0.755486408003205,
6.65621873257887));
#7372=CARTESIAN_POINT('Ctrl Pts',(0.475826092423244,-0.590582675084604,
6.6891250935537));
#7373=CARTESIAN_POINT('Ctrl Pts',(0.743223728972327,-0.165383236018042,
6.72216417731904));
#7374=CARTESIAN_POINT('Ctrl Pts',(0.687732640812107,0.335833673405217,6.75534872287688));
#7375=CARTESIAN_POINT('Ctrl Pts',(0.329161852114402,0.69473766380513,6.78868194987952));
#7376=CARTESIAN_POINT('Ctrl Pts',(-0.120255207878517,0.745235334942848,
6.81845529502086));
#7377=CARTESIAN_POINT('Ctrl Pts',(-0.467524502978826,0.57746640430216,6.84461903462784));
#7378=CARTESIAN_POINT('Ctrl Pts',(-0.674360922287096,0.318638588168112,
6.86712201294724));
#7379=CARTESIAN_POINT('Ctrl Pts',(-0.748404023106268,-0.00575219575844088,
6.88970750051041));
#7380=CARTESIAN_POINT('Ctrl Pts',(-0.674269101945005,-0.331252076513231,
6.91237414913092));
#7381=CARTESIAN_POINT('Ctrl Pts',(-0.465442485762675,-0.593360030871918,
6.93512642552479));
#7382=CARTESIAN_POINT('Ctrl Pts',(-0.162413298418938,-0.73950734230565,
6.95796516185281));
#7383=CARTESIAN_POINT('Ctrl Pts',(0.175299902719076,-0.739551441572441,
6.98089514210305));
#7384=CARTESIAN_POINT('Ctrl Pts',(0.48087309657339,-0.592568368954699,7.00391530912488));
#7385=CARTESIAN_POINT('Ctrl Pts',(0.693231099227059,-0.326542805878524,
7.02702898588934));
#7386=CARTESIAN_POINT('Ctrl Pts',(0.769520632376555,0.00680181224901938,
7.05023795575404));
#7387=CARTESIAN_POINT('Ctrl Pts',(0.693149586424791,0.341276467608696,7.07354385445611));
#7388=CARTESIAN_POINT('Ctrl Pts',(0.442928349106893,0.656453792431941,7.1008495131406));
#7389=CARTESIAN_POINT('Ctrl Pts',(-0.00655006027916784,0.814828143116751,
7.13222145322597));
#7390=CARTESIAN_POINT('Ctrl Pts',(-0.51677651805262,0.636849892039306,7.16774598353412));
#7391=CARTESIAN_POINT('Ctrl Pts',(-0.806409087124653,0.176948274600164,
7.20350474142154));
#7392=CARTESIAN_POINT('Ctrl Pts',(-0.745817965655065,-0.367012141382838,
7.2395023580954));
#7393=CARTESIAN_POINT('Ctrl Pts',(-0.356682875026977,-0.756951656680894,
7.27574101303561));
#7394=CARTESIAN_POINT('Ctrl Pts',(0.194324484528691,-0.819874060139303,
7.3122257656988));
#7395=CARTESIAN_POINT('Ctrl Pts',(0.667449116817723,-0.523027248491166,
7.34895409901446));
#7396=CARTESIAN_POINT('Ctrl Pts',(0.791458463792618,-0.170101188152833,
7.37361186684348));
#7397=CARTESIAN_POINT('Ctrl Pts',(0.791482481276893,0.00791737913227817,
7.38597037371902));
#7398=CARTESIAN_POINT('Ctrl Pts',(0.849598076317196,-0.00712734349710777,
5.50276247098815));
#7399=CARTESIAN_POINT('Ctrl Pts',(0.849572315215897,0.183814720194332,5.51601816019011));
#7400=CARTESIAN_POINT('Ctrl Pts',(0.716484451910036,0.562864504493882,5.5424997573337));
#7401=CARTESIAN_POINT('Ctrl Pts',(0.20809212706776,0.881898014322701,5.58196713633214));
#7402=CARTESIAN_POINT('Ctrl Pts',(-0.384533142466098,0.814321092392168,
5.6212091202806));
#7403=CARTESIAN_POINT('Ctrl Pts',(-0.803342488001547,0.394693505033448,
5.66020880663821));
#7404=CARTESIAN_POINT('Ctrl Pts',(-0.868627634713463,-0.190973266163329,
5.69896909964657));
#7405=CARTESIAN_POINT('Ctrl Pts',(-0.556653040774226,-0.686349150395686,
5.7374846668518));
#7406=CARTESIAN_POINT('Ctrl Pts',(-0.00707997145394115,-0.878014145711534,
5.77575459287924));
#7407=CARTESIAN_POINT('Ctrl Pts',(0.436900544149483,-0.72169954588876,5.80673549990624));
#7408=CARTESIAN_POINT('Ctrl Pts',(0.671606542222444,-0.467350263792894,
5.83056225412086));
#7409=CARTESIAN_POINT('Ctrl Pts',(0.813155385970533,-0.1750292179711,5.85292188205288));
#7410=CARTESIAN_POINT('Ctrl Pts',(0.812540057938428,0.242883178054026,5.88074814557167));
#7411=CARTESIAN_POINT('Ctrl Pts',(0.554998700939117,0.6202772367454,5.91117655608676));
#7412=CARTESIAN_POINT('Ctrl Pts',(0.189304493774159,0.795493011487289,5.93869516979536));
#7413=CARTESIAN_POINT('Ctrl Pts',(-0.173712239990491,0.795504865118224,
5.96335163063203));
#7414=CARTESIAN_POINT('Ctrl Pts',(-0.499345414071431,0.638313353697133,
5.98789731654311));
#7415=CARTESIAN_POINT('Ctrl Pts',(-0.72356068389146,0.356867037202337,6.01233388291633));
#7416=CARTESIAN_POINT('Ctrl Pts',(-0.803163168357719,0.00747357176146625,
6.03666105392709));
#7417=CARTESIAN_POINT('Ctrl Pts',(-0.736797982336716,-0.28222992698738,
6.05684360012597));
#7418=CARTESIAN_POINT('Ctrl Pts',(-0.612891815719577,-0.479031268493863,
6.07293511022899));
#7419=CARTESIAN_POINT('Ctrl Pts',(-0.448917230819194,-0.643222296978376,
6.08899082487842));
#7420=CARTESIAN_POINT('Ctrl Pts',(-0.18345184155449,-0.770972157981274,
6.10899459772628));
#7421=CARTESIAN_POINT('Ctrl Pts',(0.168509519247147,-0.770779631725406,
6.1328926650123));
#7422=CARTESIAN_POINT('Ctrl Pts',(0.484258307101598,-0.618569501699951,
6.15668614964677));
#7423=CARTESIAN_POINT('Ctrl Pts',(0.7014559478794,-0.345739709198507,6.18037560572192));
#7424=CARTESIAN_POINT('Ctrl Pts',(0.787759201210554,0.0307483449030446,
6.20658402952268));
#7425=CARTESIAN_POINT('Ctrl Pts',(0.660297100374137,0.44205148705441,6.23526827245269));
#7426=CARTESIAN_POINT('Ctrl Pts',(0.29489586174265,0.733477282971818,6.2663838499292));
#7427=CARTESIAN_POINT('Ctrl Pts',(-0.168647261234911,0.767641847640704,
6.2973293246475));
#7428=CARTESIAN_POINT('Ctrl Pts',(-0.568727882191308,0.536181820843462,
6.32810567535681));
#7429=CARTESIAN_POINT('Ctrl Pts',(-0.768048251626985,0.121961889290114,
6.35871685457357));
#7430=CARTESIAN_POINT('Ctrl Pts',(-0.697107833504566,-0.349296397819721,
6.39043824166099));
#7431=CARTESIAN_POINT('Ctrl Pts',(-0.344045555812211,-0.701995892428354,
6.42325363059534));
#7432=CARTESIAN_POINT('Ctrl Pts',(0.110773521189623,-0.752235352072163,
6.45337778122228));
#7433=CARTESIAN_POINT('Ctrl Pts',(0.458965638454581,-0.583886825258837,
6.47961716649731));
#7434=CARTESIAN_POINT('Ctrl Pts',(0.664381883487217,-0.325864755846388,
6.50203114286227));
#7435=CARTESIAN_POINT('Ctrl Pts',(0.750332653299937,0.0485776788759206,
6.52809351690923));
#7436=CARTESIAN_POINT('Ctrl Pts',(0.601674226486008,0.473897649396157,6.55776163974272));
#7437=CARTESIAN_POINT('Ctrl Pts',(0.173613673117217,0.742348086642931,6.59098287751551));
#7438=CARTESIAN_POINT('Ctrl Pts',(-0.3258350440189,0.685649541287933,6.62406030334558));
#7439=CARTESIAN_POINT('Ctrl Pts',(-0.679731238547397,0.331354382468774,
6.65700275666622));
#7440=CARTESIAN_POINT('Ctrl Pts',(-0.735255898447251,-0.164397347346024,
6.6898206739066));
#7441=CARTESIAN_POINT('Ctrl Pts',(-0.470558029977308,-0.585159244984441,
6.7225241569716));
#7442=CARTESIAN_POINT('Ctrl Pts',(-0.00278192751448173,-0.748569972495831,
6.75512382817215));
#7443=CARTESIAN_POINT('Ctrl Pts',(0.46350519113553,-0.58518407843876,6.78763042208935));
#7444=CARTESIAN_POINT('Ctrl Pts',(0.725410474458316,-0.167706567477984,
6.82005514647598));
#7445=CARTESIAN_POINT('Ctrl Pts',(0.670774587918448,0.320804047707368,6.85240545447397));
#7446=CARTESIAN_POINT('Ctrl Pts',(0.323092957157568,0.668041717311718,6.88470045447928));
#7447=CARTESIAN_POINT('Ctrl Pts',(-0.109494451463983,0.716184576245998,
6.91336373465137));
#7448=CARTESIAN_POINT('Ctrl Pts',(-0.44188826662967,0.555407233522295,6.93841735921765));
#7449=CARTESIAN_POINT('Ctrl Pts',(-0.639012403336459,0.308500858246645,
6.95988071793453));
#7450=CARTESIAN_POINT('Ctrl Pts',(-0.709192507424316,0.00040641570270789,
6.98133136104379));
#7451=CARTESIAN_POINT('Ctrl Pts',(-0.638918625948615,-0.307487189319304,
7.00277862675193));
#7452=CARTESIAN_POINT('Ctrl Pts',(-0.442028652642433,-0.554399048208452,
7.02422233485342));
#7453=CARTESIAN_POINT('Ctrl Pts',(-0.157482946544586,-0.691481626684627,
7.0456683320825));
#7454=CARTESIAN_POINT('Ctrl Pts',(0.15835851542768,-0.691398914091788,7.06711532573104));
#7455=CARTESIAN_POINT('Ctrl Pts',(0.44307547960184,-0.554307235545146,7.08857226527194));
#7456=CARTESIAN_POINT('Ctrl Pts',(0.64018584092255,-0.307192493791569,7.11004002498397));
#7457=CARTESIAN_POINT('Ctrl Pts',(0.71067332605218,0.00132671397574847,
7.13152214083118));
#7458=CARTESIAN_POINT('Ctrl Pts',(0.640127181409651,0.309809306958141,7.15302225181439));
#7459=CARTESIAN_POINT('Ctrl Pts',(0.409965562319378,0.59950154513597,7.1781297331652));
#7460=CARTESIAN_POINT('Ctrl Pts',(-0.00180430761257666,0.744250295435473,
7.20686838534354));
#7461=CARTESIAN_POINT('Ctrl Pts',(-0.46689999412445,0.581628177637233,7.23926440850474));
#7462=CARTESIAN_POINT('Ctrl Pts',(-0.729602505011613,0.163869023223047,
7.27173917712393));
#7463=CARTESIAN_POINT('Ctrl Pts',(-0.674485616164893,-0.328104186907804,
7.3043020520652));
#7464=CARTESIAN_POINT('Ctrl Pts',(-0.32358572160231,-0.679299557613987,
7.33696613118188));
#7465=CARTESIAN_POINT('Ctrl Pts',(0.171370920939519,-0.735610678055291,
7.36973771478191));
#7466=CARTESIAN_POINT('Ctrl Pts',(0.594929256360531,-0.469509634858928,
7.40263639340595));
#7467=CARTESIAN_POINT('Ctrl Pts',(0.705563583847616,-0.154509464242322,
7.42464584593578));
#7468=CARTESIAN_POINT('Ctrl Pts',(0.705585033709163,0.00447777927316105,
7.4356831493591));
#7469=CARTESIAN_POINT('Ctrl Pts',(0.911787311372316,-0.00175313599507732,
5.42547035947661));
#7470=CARTESIAN_POINT('Ctrl Pts',(0.911759679946333,0.203051830949188,5.43968844708048));
#7471=CARTESIAN_POINT('Ctrl Pts',(0.768907437119982,0.61071591344494,5.46816718430648));
#7472=CARTESIAN_POINT('Ctrl Pts',(0.220284165601068,0.955502366817236,5.51077805671262));
#7473=CARTESIAN_POINT('Ctrl Pts',(-0.422243656323184,0.882710139668278,
5.55332558349325));
#7474=CARTESIAN_POINT('Ctrl Pts',(-0.878386039542625,0.426289581625414,
5.5957765844892));
#7475=CARTESIAN_POINT('Ctrl Pts',(-0.950141006447777,-0.213553723589873,
5.63813025439539));
#7476=CARTESIAN_POINT('Ctrl Pts',(-0.60835728725253,-0.757014115469509,
5.68037224924266));
#7477=CARTESIAN_POINT('Ctrl Pts',(-0.00366338310403281,-0.968314430281517,
5.72249300107482));
#7478=CARTESIAN_POINT('Ctrl Pts',(0.486718248881734,-0.795970516833383,
5.75670865791863));
#7479=CARTESIAN_POINT('Ctrl Pts',(0.74653021351722,-0.514477549037207,5.78308078863264));
#7480=CARTESIAN_POINT('Ctrl Pts',(0.903446118847398,-0.190511009717507,
5.80786424281498));
#7481=CARTESIAN_POINT('Ctrl Pts',(0.90295145376886,0.273634535370419,5.8387700025228));
#7482=CARTESIAN_POINT('Ctrl Pts',(0.616343546706946,0.693954207986666,5.87265196790731));
#7483=CARTESIAN_POINT('Ctrl Pts',(0.208328450290096,0.889559871552857,5.90335942490417));
#7484=CARTESIAN_POINT('Ctrl Pts',(-0.197431208021256,0.889652469467467,
5.93091996947637));
#7485=CARTESIAN_POINT('Ctrl Pts',(-0.562029250439909,0.713737268348937,
5.95840063131195));
#7486=CARTESIAN_POINT('Ctrl Pts',(-0.813494233574056,0.39820149627948,5.98580131723829));
#7487=CARTESIAN_POINT('Ctrl Pts',(-0.902946074851847,0.0058870464447316,
6.01311843029465));
#7488=CARTESIAN_POINT('Ctrl Pts',(-0.828377509677636,-0.319866751453087,
6.03581174060078));
#7489=CARTESIAN_POINT('Ctrl Pts',(-0.688936970150508,-0.541360820821501,
6.05392170180393));
#7490=CARTESIAN_POINT('Ctrl Pts',(-0.504293132651573,-0.726263454623667,
6.07200206864918));
#7491=CARTESIAN_POINT('Ctrl Pts',(-0.205118119105362,-0.870286210128437,
6.0945471479209));
#7492=CARTESIAN_POINT('Ctrl Pts',(0.191971983732839,-0.870117700265186,
6.12150897978661));
#7493=CARTESIAN_POINT('Ctrl Pts',(0.548553466642107,-0.698273117288175,
6.14837718076188));
#7494=CARTESIAN_POINT('Ctrl Pts',(0.794052616995502,-0.389950825708538,
6.17514969693223));
#7495=CARTESIAN_POINT('Ctrl Pts',(0.891698024550524,0.0358312226908213,
6.20478886300642));
#7496=CARTESIAN_POINT('Ctrl Pts',(0.74749095040922,0.501334011480795,6.23725086378811));
#7497=CARTESIAN_POINT('Ctrl Pts',(0.333743343393983,0.831378563455359,6.27248425191807));
#7498=CARTESIAN_POINT('Ctrl Pts',(-0.19134387466354,0.870105625426578,6.3075348767601));
#7499=CARTESIAN_POINT('Ctrl Pts',(-0.644616547373273,0.607881105022717,
6.34239973374175));
#7500=CARTESIAN_POINT('Ctrl Pts',(-0.870417110421222,0.138612855199806,
6.37707657725051));
#7501=CARTESIAN_POINT('Ctrl Pts',(-0.790048775469081,-0.39510788351932,
6.41299953612703));
#7502=CARTESIAN_POINT('Ctrl Pts',(-0.390383204661376,-0.794274173322802,
6.45013660062964));
#7503=CARTESIAN_POINT('Ctrl Pts',(0.123964069137483,-0.851002982786416,
6.48419818277685));
#7504=CARTESIAN_POINT('Ctrl Pts',(0.517349958215306,-0.660759929294058,
6.51384272570464));
#7505=CARTESIAN_POINT('Ctrl Pts',(0.749191592206741,-0.369479150376496,
6.53914157276564));
#7506=CARTESIAN_POINT('Ctrl Pts',(0.846067098454331,0.052769037404062,6.56852738290555));
#7507=CARTESIAN_POINT('Ctrl Pts',(0.678541487051601,0.531594017531224,6.60192411587722));
#7508=CARTESIAN_POINT('Ctrl Pts',(0.197445708687755,0.833056774682923,6.63924640568331));
#7509=CARTESIAN_POINT('Ctrl Pts',(-0.362407034535075,0.76926077023711,6.67631865996902));
#7510=CARTESIAN_POINT('Ctrl Pts',(-0.757891257853047,0.372960662447378,
6.7131423125874));
#7511=CARTESIAN_POINT('Ctrl Pts',(-0.819502812158925,-0.17971389368945,
6.74971854734871));
#7512=CARTESIAN_POINT('Ctrl Pts',(-0.525117958852971,-0.647082052916212,
6.78604945080241));
#7513=CARTESIAN_POINT('Ctrl Pts',(-0.00706009915885147,-0.827706145589558,
6.82213749402266));
#7514=CARTESIAN_POINT('Ctrl Pts',(0.507168732938518,-0.647142083318005,
6.85798569667506));
#7515=CARTESIAN_POINT('Ctrl Pts',(0.794559460318739,-0.188312585352296,
6.89359746949419));
#7516=CARTESIAN_POINT('Ctrl Pts',(0.734412407851191,0.346047384757273,6.92898046138837));
#7517=CARTESIAN_POINT('Ctrl Pts',(0.35554627917015,0.723799648271606,6.96413145325235));
#7518=CARTESIAN_POINT('Ctrl Pts',(-0.113206435891536,0.775602232806529,
6.99517934888198));
#7519=CARTESIAN_POINT('Ctrl Pts',(-0.471799040782441,0.601968214167806,
7.0222090326148));
#7520=CARTESIAN_POINT('Ctrl Pts',(-0.6836661147338,0.336404243341276,7.04528069450069));
#7521=CARTESIAN_POINT('Ctrl Pts',(-0.758726003996092,0.0062400461075705,
7.06826344122686));
#7522=CARTESIAN_POINT('Ctrl Pts',(-0.6835849590214,-0.322409867084328,7.09115224380289));
#7523=CARTESIAN_POINT('Ctrl Pts',(-0.474072442185209,-0.584919976115439,
7.11395355010067));
#7524=CARTESIAN_POINT('Ctrl Pts',(-0.172560181698569,-0.730020088066619,
7.13666650878931));
#7525=CARTESIAN_POINT('Ctrl Pts',(0.16078217307758,-0.729778328929261,7.15929927954856));
#7526=CARTESIAN_POINT('Ctrl Pts',(0.459989212508115,-0.585545816121325,
7.18184723354721));
#7527=CARTESIAN_POINT('Ctrl Pts',(0.666223161118391,-0.32674631555655,7.20431603435277));
#7528=CARTESIAN_POINT('Ctrl Pts',(0.739554158501798,-0.00504686561265504,
7.22670799379599));
#7529=CARTESIAN_POINT('Ctrl Pts',(0.666159558065311,0.315205418031567,7.24902537021377));
#7530=CARTESIAN_POINT('Ctrl Pts',(0.428020561210259,0.614621005636118,7.27497954766194));
#7531=CARTESIAN_POINT('Ctrl Pts',(0.00440289337514439,0.763018006049135,
7.30452179484735));
#7532=CARTESIAN_POINT('Ctrl Pts',(-0.470624128322024,0.596319364034835,
7.33761244678054));
#7533=CARTESIAN_POINT('Ctrl Pts',(-0.736811683564632,0.171965979607826,
7.37056624676418));
#7534=CARTESIAN_POINT('Ctrl Pts',(-0.68068387352667,-0.324086643305756,
7.4033919913947));
#7535=CARTESIAN_POINT('Ctrl Pts',(-0.328791217341046,-0.675487864461335,
7.43610391008164));
#7536=CARTESIAN_POINT('Ctrl Pts',(0.163774412047771,-0.731012482418632,
7.4687018632077));
#7537=CARTESIAN_POINT('Ctrl Pts',(0.582152961317522,-0.467440680790944,
7.50121977146286));
#7538=CARTESIAN_POINT('Ctrl Pts',(0.690380552641563,-0.158133439986746,
7.52281364669809));
#7539=CARTESIAN_POINT('Ctrl Pts',(0.690401574315868,-0.00231993767140268,
7.53363062084317));
#7540=CARTESIAN_POINT('Ctrl Pts',(0.889359432826132,0.00495444760725769,
5.32880713791624));
#7541=CARTESIAN_POINT('Ctrl Pts',(0.889332447864276,0.204967802847453,5.34269257951066));
#7542=CARTESIAN_POINT('Ctrl Pts',(0.750004347575518,0.603672713614473,5.37053043303203));
#7543=CARTESIAN_POINT('Ctrl Pts',(0.21096706922133,0.94314460394843,5.41241969183905));
#7544=CARTESIAN_POINT('Ctrl Pts',(-0.423963274156834,0.87171349864309,5.45445132266662));
#7545=CARTESIAN_POINT('Ctrl Pts',(-0.877374490363263,0.418799407840054,
5.4966071161887));
#7546=CARTESIAN_POINT('Ctrl Pts',(-0.949545774103564,-0.219892556824646,
5.53888079270843));
#7547=CARTESIAN_POINT('Ctrl Pts',(-0.607068575689537,-0.765494054358749,
5.58125986451715));
#7548=CARTESIAN_POINT('Ctrl Pts',(0.00261167844658479,-0.97913119777945,
5.62373519298684));
#7549=CARTESIAN_POINT('Ctrl Pts',(0.499852533620251,-0.8048463257254,5.65841239967706));
#7550=CARTESIAN_POINT('Ctrl Pts',(0.764265215589788,-0.518466038803169,
5.68524380080038));
#7551=CARTESIAN_POINT('Ctrl Pts',(0.924328881255501,-0.188150671604858,
5.71051448038525));
#7552=CARTESIAN_POINT('Ctrl Pts',(0.924132430512447,0.286757902074732,5.74213409224145));
#7553=CARTESIAN_POINT('Ctrl Pts',(0.62986087869606,0.718937325916808,5.77695468815655));
#7554=CARTESIAN_POINT('Ctrl Pts',(0.208953775300158,0.920912997464213,5.80863418802737));
#7555=CARTESIAN_POINT('Ctrl Pts',(-0.211068988110463,0.921157282542793,
5.83716174516452));
#7556=CARTESIAN_POINT('Ctrl Pts',(-0.589810577699277,0.738585626106938,
5.86570218738055));
#7557=CARTESIAN_POINT('Ctrl Pts',(-0.85194552766839,0.409898301969846,5.89425134138179));
#7558=CARTESIAN_POINT('Ctrl Pts',(-0.945597945878367,-0.000176678256206242,
5.92280607763768));
#7559=CARTESIAN_POINT('Ctrl Pts',(-0.867511729419428,-0.341824865852328,
5.94660339370044));
#7560=CARTESIAN_POINT('Ctrl Pts',(-0.720944780593085,-0.574681060925877,
5.96564071682787));
#7561=CARTESIAN_POINT('Ctrl Pts',(-0.526555141270467,-0.769375552079073,
5.98467700523746));
#7562=CARTESIAN_POINT('Ctrl Pts',(-0.210870756052851,-0.921475670946048,
6.00846936790163));
#7563=CARTESIAN_POINT('Ctrl Pts',(0.209506448294534,-0.921438779399368,
6.03701193615958));
#7564=CARTESIAN_POINT('Ctrl Pts',(0.588220824730041,-0.739083885420811,
6.0655428661009));
#7565=CARTESIAN_POINT('Ctrl Pts',(0.849810718286318,-0.410765395052392,
6.09405857275419));
#7566=CARTESIAN_POINT('Ctrl Pts',(0.95427567990068,0.0440511715684175,6.12572236137368));
#7567=CARTESIAN_POINT('Ctrl Pts',(0.799967960952214,0.54314825140328,6.16052078866217));
#7568=CARTESIAN_POINT('Ctrl Pts',(0.354946991113063,0.898546473402006,6.19843574858538));
#7569=CARTESIAN_POINT('Ctrl Pts',(-0.212199085766547,0.940684954588202,
6.23629684514792));
#7570=CARTESIAN_POINT('Ctrl Pts',(-0.703732454340991,0.656671161576527,
6.27409476897982));
#7571=CARTESIAN_POINT('Ctrl Pts',(-0.949639640621547,0.146281182681,6.31182133692065));
#7572=CARTESIAN_POINT('Ctrl Pts',(-0.862200374710721,-0.436390813484725,
6.35103882924841));
#7573=CARTESIAN_POINT('Ctrl Pts',(-0.424615550503731,-0.87396308504598,
6.39172839424829));
#7574=CARTESIAN_POINT('Ctrl Pts',(0.140875049279472,-0.936660006455991,
6.42918239638723));
#7575=CARTESIAN_POINT('Ctrl Pts',(0.574670287621894,-0.727011014446981,
6.46186903203473));
#7576=CARTESIAN_POINT('Ctrl Pts',(0.83093266790137,-0.405200393190354,6.48982632103455));
#7577=CARTESIAN_POINT('Ctrl Pts',(0.938317766588939,0.0623494789078903,
6.52236975513327));
#7578=CARTESIAN_POINT('Ctrl Pts',(0.752579540678534,0.594055251251905,6.55945509994811));
#7579=CARTESIAN_POINT('Ctrl Pts',(0.217059284541729,0.929973502219806,6.60101727981861));
#7580=CARTESIAN_POINT('Ctrl Pts',(-0.408026785252189,0.859019100893442,
6.6424136299843));
#7581=CARTESIAN_POINT('Ctrl Pts',(-0.850845977716372,0.415638179906151,
6.68363494790014));
#7582=CARTESIAN_POINT('Ctrl Pts',(-0.920184777472661,-0.204329024249146,
6.72467349392044));
#7583=CARTESIAN_POINT('Ctrl Pts',(-0.589428074185655,-0.729814282912527,
6.76552142650441));
#7584=CARTESIAN_POINT('Ctrl Pts',(-0.00604978450581677,-0.933394312826398,
6.80617154371966));
#7585=CARTESIAN_POINT('Ctrl Pts',(0.57404869025302,-0.72985742835735,6.84661700406497));
#7586=CARTESIAN_POINT('Ctrl Pts',(0.898783211561984,-0.211649435517353,
6.8868516259356));
#7587=CARTESIAN_POINT('Ctrl Pts',(0.830853561486015,0.392570978289185,6.92686564614092));
#7588=CARTESIAN_POINT('Ctrl Pts',(0.402102843122056,0.820171632165624,6.96666187541315));
#7589=CARTESIAN_POINT('Ctrl Pts',(-0.128752136760593,0.87885181573823,7.0018337119622));
#7590=CARTESIAN_POINT('Ctrl Pts',(-0.534933891924655,0.682185839564183,
7.03245541763881));
#7591=CARTESIAN_POINT('Ctrl Pts',(-0.774943785493673,0.381327511531892,
7.05860032562784));
#7592=CARTESIAN_POINT('Ctrl Pts',(-0.859966110515312,0.00734177845082202,
7.08463607645075));
#7593=CARTESIAN_POINT('Ctrl Pts',(-0.774831422913684,-0.364904312674865,
7.11056853328824));
#7594=CARTESIAN_POINT('Ctrl Pts',(-0.537583138232402,-0.662143756003773,
7.13639250543407));
#7595=CARTESIAN_POINT('Ctrl Pts',(-0.196279169025999,-0.826362279426242,
7.16211006197668));
#7596=CARTESIAN_POINT('Ctrl Pts',(0.180788904256726,-0.82607059745876,7.18771480491698));
#7597=CARTESIAN_POINT('Ctrl Pts',(0.519038634180724,-0.662978803853832,
7.21321277550856));
#7598=CARTESIAN_POINT('Ctrl Pts',(0.751978439186691,-0.370613914749894,
7.23860036966167));
#7599=CARTESIAN_POINT('Ctrl Pts',(0.834701683971329,-0.00754650688657486,
7.26387733624003));
#7600=CARTESIAN_POINT('Ctrl Pts',(0.751920252216622,0.353483451503403,7.28904368273798));
#7601=CARTESIAN_POINT('Ctrl Pts',(0.483730036422595,0.690590593695916,7.31827398545647));
#7602=CARTESIAN_POINT('Ctrl Pts',(0.00742785048027893,0.857265989116031,
7.35149921639049));
#7603=CARTESIAN_POINT('Ctrl Pts',(-0.525293231887737,0.670073438058683,
7.38862588821794));
#7604=CARTESIAN_POINT('Ctrl Pts',(-0.822869944746703,0.195197072733832,
7.42550481928346));
#7605=CARTESIAN_POINT('Ctrl Pts',(-0.759959606004209,-0.358130855720698,
7.46213543363099));
#7606=CARTESIAN_POINT('Ctrl Pts',(-0.368415214766548,-0.748693330694505,
7.49852208898732));
#7607=CARTESIAN_POINT('Ctrl Pts',(0.177541916017237,-0.809855769006471,
7.53466251134493));
#7608=CARTESIAN_POINT('Ctrl Pts',(0.639295990646259,-0.518615892317653,
7.57056942797824));
#7609=CARTESIAN_POINT('Ctrl Pts',(0.758201052838224,-0.178255309934477,
7.59433715581631));
#7610=CARTESIAN_POINT('Ctrl Pts',(0.758224108327783,-0.00736708650145173,
7.60620065587956));
#7611=CARTESIAN_POINT('Ctrl Pts',(0.829918995390605,0.00692962491070555,
5.30024010712383));
#7612=CARTESIAN_POINT('Ctrl Pts',(0.829893790259993,0.193750817013165,5.31320971482039));
#7613=CARTESIAN_POINT('Ctrl Pts',(0.699822285583035,0.566145381882556,5.3392101566049));
#7614=CARTESIAN_POINT('Ctrl Pts',(0.195323515234371,0.88416117171195,5.37842883489126));
#7615=CARTESIAN_POINT('Ctrl Pts',(-0.400343151138505,0.817346474568011,
5.41785865980122));
#7616=CARTESIAN_POINT('Ctrl Pts',(-0.826817727686594,0.391700174990477,
5.4574958434249));
#7617=CARTESIAN_POINT('Ctrl Pts',(-0.895091678603364,-0.210180305596499,
5.49733544534094));
#7618=CARTESIAN_POINT('Ctrl Pts',(-0.571783532988076,-0.72574941013594,
5.53737192540201));
#7619=CARTESIAN_POINT('Ctrl Pts',(0.00554627097635579,-0.928352383739425,
5.57760056939562));
#7620=CARTESIAN_POINT('Ctrl Pts',(0.477799679854192,-0.76307476144334,5.61052921806703));
#7621=CARTESIAN_POINT('Ctrl Pts',(0.729410852594162,-0.490616169914011,
5.63605789108779));
#7622=CARTESIAN_POINT('Ctrl Pts',(0.881919476817548,-0.175979128010471,
5.66013043243701));
#7623=CARTESIAN_POINT('Ctrl Pts',(0.881906152444497,0.277265930526209,5.69030700929344));
#7624=CARTESIAN_POINT('Ctrl Pts',(0.600514890488868,0.690886371812261,5.72362170442843));
#7625=CARTESIAN_POINT('Ctrl Pts',(0.196921477412404,0.884675277260858,5.75399952860311));
#7626=CARTESIAN_POINT('Ctrl Pts',(-0.206656190820974,0.885009407611865,
5.78140796402136));
#7627=CARTESIAN_POINT('Ctrl Pts',(-0.571352525906284,0.709312471916405,
5.80888598178339));
#7628=CARTESIAN_POINT('Ctrl Pts',(-0.824322784093117,0.39228222278969,5.8364255516956));
#7629=CARTESIAN_POINT('Ctrl Pts',(-0.914955919505048,-0.00412326864883124,
5.86402777825679));
#7630=CARTESIAN_POINT('Ctrl Pts',(-0.839394814319228,-0.335102288993869,
5.88707765903504));
#7631=CARTESIAN_POINT('Ctrl Pts',(-0.697194784237861,-0.561053925833896,
5.90554855730548));
#7632=CARTESIAN_POINT('Ctrl Pts',(-0.508394551716055,-0.75017609097147,
5.9240379575655));
#7633=CARTESIAN_POINT('Ctrl Pts',(-0.201331843767861,-0.89822223947356,
5.94717992736717));
#7634=CARTESIAN_POINT('Ctrl Pts',(0.208503775368862,-0.898293333883727,
5.97500361673599));
#7635=CARTESIAN_POINT('Ctrl Pts',(0.578566181754719,-0.72022509709185,6.00287494476189));
#7636=CARTESIAN_POINT('Ctrl Pts',(0.834785028018541,-0.398807815817064,
6.03079323532));
#7637=CARTESIAN_POINT('Ctrl Pts',(0.937421618538533,0.0474693145637866,
6.06185942553353));
#7638=CARTESIAN_POINT('Ctrl Pts',(0.785808706512713,0.53858289651246,6.09609235737173));
#7639=CARTESIAN_POINT('Ctrl Pts',(0.346833476768302,0.889498241929319,6.13350258691761));
#7640=CARTESIAN_POINT('Ctrl Pts',(-0.214450953963022,0.931459250732699,
6.17096335002368));
#7641=CARTESIAN_POINT('Ctrl Pts',(-0.702523232936964,0.649744126672763,
6.20847735887153));
#7642=CARTESIAN_POINT('Ctrl Pts',(-0.947620032703892,0.141637172177686,
6.24603852533507));
#7643=CARTESIAN_POINT('Ctrl Pts',(-0.860569087705711,-0.440346323520561,
6.28520072180747));
#7644=CARTESIAN_POINT('Ctrl Pts',(-0.422417509108382,-0.879011958721694,
6.32595508450303));
#7645=CARTESIAN_POINT('Ctrl Pts',(0.146053510149855,-0.942361769529175,
6.36359784749923));
#7646=CARTESIAN_POINT('Ctrl Pts',(0.583529811691089,-0.731092224974979,
6.39655251871174));
#7647=CARTESIAN_POINT('Ctrl Pts',(0.842579028174264,-0.405926837413371,
6.42480144817265));
#7648=CARTESIAN_POINT('Ctrl Pts',(0.951487177832284,0.0675991994034292,
6.45775864234018));
#7649=CARTESIAN_POINT('Ctrl Pts',(0.763141746082221,0.607725575505774,6.49541116932488));
#7650=CARTESIAN_POINT('Ctrl Pts',(0.217574487524898,0.950392778021499,6.53775763542001));
#7651=CARTESIAN_POINT('Ctrl Pts',(-0.42166740973873,0.878191572890031,6.58007504544765));
#7652=CARTESIAN_POINT('Ctrl Pts',(-0.876250398231941,0.423545215383675,
6.62235503675604));
#7653=CARTESIAN_POINT('Ctrl Pts',(-0.947987096499237,-0.21459643925478,
6.6645859298645));
#7654=CARTESIAN_POINT('Ctrl Pts',(-0.606705076713124,-0.757473932422971,
6.70675774894366));
#7655=CARTESIAN_POINT('Ctrl Pts',(-0.00241202776964925,-0.968727997454768,
6.74885991888449));
#7656=CARTESIAN_POINT('Ctrl Pts',(0.600624482148029,-0.757509613558942,
6.79088237303874));
#7657=CARTESIAN_POINT('Ctrl Pts',(0.939452177122731,-0.217421016410473,
6.8328144749144));
#7658=CARTESIAN_POINT('Ctrl Pts',(0.868758799747721,0.414536277515111,6.87465507197778));
#7659=CARTESIAN_POINT('Ctrl Pts',(0.419290549746345,0.863247184920627,6.91637647714826));
#7660=CARTESIAN_POINT('Ctrl Pts',(-0.139084650191804,0.925265402913614,
6.95335818017224));
#7661=CARTESIAN_POINT('Ctrl Pts',(-0.567454545740675,0.717965354424563,
6.98564100520883));
#7662=CARTESIAN_POINT('Ctrl Pts',(-0.821064769263926,0.400211556185252,
7.0132490098583));
#7663=CARTESIAN_POINT('Ctrl Pts',(-0.91112933929112,0.00438963293201363,
7.04080231652177));
#7664=CARTESIAN_POINT('Ctrl Pts',(-0.820966778853315,-0.390275853878312,
7.0682856755789));
#7665=CARTESIAN_POINT('Ctrl Pts',(-0.569057996064222,-0.706001271167066,
7.09570447796615));
#7666=CARTESIAN_POINT('Ctrl Pts',(-0.206027274734066,-0.880764451318613,
7.1230513221731));
#7667=CARTESIAN_POINT('Ctrl Pts',(0.195812674813625,-0.880515195886687,
7.15033395522949));
#7668=CARTESIAN_POINT('Ctrl Pts',(0.556847139748695,-0.706517914293179,
7.17753857633508));
#7669=CARTESIAN_POINT('Ctrl Pts',(0.805895709935206,-0.394032847218828,
7.20466842663578));
#7670=CARTESIAN_POINT('Ctrl Pts',(0.894511398596212,-0.00535918267020315,
7.2317212151674));
#7671=CARTESIAN_POINT('Ctrl Pts',(0.805810304168001,0.381721934163946,7.25869451527825));
#7672=CARTESIAN_POINT('Ctrl Pts',(0.517921324180488,0.743697104768732,7.29007024661223));
#7673=CARTESIAN_POINT('Ctrl Pts',(0.00578604455006559,0.923078227892816,
7.32578329054371));
#7674=CARTESIAN_POINT('Ctrl Pts',(-0.568243145767641,0.721567999099011,
7.3657709938243));
#7675=CARTESIAN_POINT('Ctrl Pts',(-0.889554950114489,0.209118291781916,
7.40555959496073));
#7676=CARTESIAN_POINT('Ctrl Pts',(-0.821710123582801,-0.38904286980981,
7.44514503289073));
#7677=CARTESIAN_POINT('Ctrl Pts',(-0.397947019918738,-0.811956407468429,
7.48452302388204));
#7678=CARTESIAN_POINT('Ctrl Pts',(0.193792979174468,-0.878334837234862,
7.52368670026048));
#7679=CARTESIAN_POINT('Ctrl Pts',(0.694889984053186,-0.562420176620936,
7.56263844726097));
#7680=CARTESIAN_POINT('Ctrl Pts',(0.823996878593897,-0.192605752293447,
7.58845159102269));
#7681=CARTESIAN_POINT('Ctrl Pts',(0.824021914564924,-0.00703811992170032,
7.60133417341575));
#7682=CARTESIAN_POINT('Ctrl Pts',(0.799999065628721,0.00692558823944229,
5.30024010712383));
#7683=CARTESIAN_POINT('Ctrl Pts',(0.799974755250737,0.187114846749742,5.31274930893178));
#7684=CARTESIAN_POINT('Ctrl Pts',(0.674578200671659,0.546127076651831,5.33781512365923));
#7685=CARTESIAN_POINT('Ctrl Pts',(0.187998995393781,0.852903359039399,5.37564381521248));
#7686=CARTESIAN_POINT('Ctrl Pts',(-0.386721866921525,0.788448388841122,
5.41368605209984));
#7687=CARTESIAN_POINT('Ctrl Pts',(-0.7983994419892,0.377627224111744,5.45194644400096));
#7688=CARTESIAN_POINT('Ctrl Pts',(-0.864375113399524,-0.203617876612744,
5.49042055747836));
#7689=CARTESIAN_POINT('Ctrl Pts',(-0.552019639313923,-0.701812288635587,
5.52910737914477));
#7690=CARTESIAN_POINT('Ctrl Pts',(0.00615426428515267,-0.897757418326962,
5.56800374230524));
#7691=CARTESIAN_POINT('Ctrl Pts',(0.463089276607972,-0.737891299975203,
5.59986549204054));
#7692=CARTESIAN_POINT('Ctrl Pts',(0.706662565433678,-0.474149107376678,
5.62457829573124));
#7693=CARTESIAN_POINT('Ctrl Pts',(0.854347338563578,-0.169471123140589,
5.6478904398873));
#7694=CARTESIAN_POINT('Ctrl Pts',(0.854381411403854,0.269671075667267,5.67712918390586));
#7695=CARTESIAN_POINT('Ctrl Pts',(0.581578462406747,0.670744438556907,5.70943359497258));
#7696=CARTESIAN_POINT('Ctrl Pts',(0.189982000930166,0.858805851522918,5.73891161848027));
#7697=CARTESIAN_POINT('Ctrl Pts',(-0.201854620920769,0.859148371452269,
5.76552549972421));
#7698=CARTESIAN_POINT('Ctrl Pts',(-0.556170302204947,0.688486751453872,
5.79222147180784));
#7699=CARTESIAN_POINT('Ctrl Pts',(-0.802120584542054,0.380288702719923,
5.81899788702529));
#7700=CARTESIAN_POINT('Ctrl Pts',(-0.890321102734134,-0.0053444036833259,
5.84585301727138));
#7701=CARTESIAN_POINT('Ctrl Pts',(-0.816781798992104,-0.327577127496462,
5.86829638740099));
#7702=CARTESIAN_POINT('Ctrl Pts',(-0.678277859648778,-0.547664335405585,
5.88628859994389));
#7703=CARTESIAN_POINT('Ctrl Pts',(-0.494316135451619,-0.731945478665225,
5.90430550175064));
#7704=CARTESIAN_POINT('Ctrl Pts',(-0.194941007989142,-0.876310026230692,
5.92687230420244));
#7705=CARTESIAN_POINT('Ctrl Pts',(0.204945568353256,-0.876409485122255,
5.95402353339188));
#7706=CARTESIAN_POINT('Ctrl Pts',(0.566325487118899,-0.702556101088839,
5.98124373289334));
#7707=CARTESIAN_POINT('Ctrl Pts',(0.816751045229916,-0.388463305588866,
6.00853075028047));
#7708=CARTESIAN_POINT('Ctrl Pts',(0.917174982875959,0.0480250206861584,
6.03892142694837));
#7709=CARTESIAN_POINT('Ctrl Pts',(0.768829350780382,0.528866010776267,6.07244001895545));
#7710=CARTESIAN_POINT('Ctrl Pts',(0.338627495917749,0.872873034891815,6.10911095186911));
#7711=CARTESIAN_POINT('Ctrl Pts',(-0.212178222814091,0.914151313349766,
6.14588130840082));
#7712=CARTESIAN_POINT('Ctrl Pts',(-0.691759933067223,0.637451614256161,
6.18274515756461));
#7713=CARTESIAN_POINT('Ctrl Pts',(-0.932934482256533,0.137697594997002,
6.21969639210087));
#7714=CARTESIAN_POINT('Ctrl Pts',(-0.84730393945114,-0.435496308403701,
6.25827178793966));
#7715=CARTESIAN_POINT('Ctrl Pts',(-0.415273257958933,-0.868240176171726,
6.29847623644814));
#7716=CARTESIAN_POINT('Ctrl Pts',(0.146189896678077,-0.930950222024402,
6.33566388079779));
#7717=CARTESIAN_POINT('Ctrl Pts',(0.578787425776111,-0.722091726547751,
6.36825221458814));
#7718=CARTESIAN_POINT('Ctrl Pts',(0.835229259505866,-0.400278931762148,
6.3962159259868));
#7719=CARTESIAN_POINT('Ctrl Pts',(0.943177486850013,0.0688606453452641,
6.42887288667825));
#7720=CARTESIAN_POINT('Ctrl Pts',(0.756462512495389,0.604750444420971,6.46623690685835));
#7721=CARTESIAN_POINT('Ctrl Pts',(0.214509054547464,0.945343920852135,6.50831791566041));
#7722=CARTESIAN_POINT('Ctrl Pts',(-0.421585054233784,0.873670673138226,
6.55043539297339));
#7723=CARTESIAN_POINT('Ctrl Pts',(-0.874725713994987,0.420703846750279,
6.59257924943873));
#7724=CARTESIAN_POINT('Ctrl Pts',(-0.946491736933492,-0.216206220818672,
6.63473932973225));
#7725=CARTESIAN_POINT('Ctrl Pts',(-0.605472064685913,-0.758979181442101,
6.67690544450194));
#7726=CARTESIAN_POINT('Ctrl Pts',(-0.000509641250504898,-0.970641038681315,
6.71906739492544));
#7727=CARTESIAN_POINT('Ctrl Pts',(0.604236817182525,-0.758999928674301,
6.76121498571335));
#7728=CARTESIAN_POINT('Ctrl Pts',(0.944676427167983,-0.216670516455945,
6.80333805746961));
#7729=CARTESIAN_POINT('Ctrl Pts',(0.873719648783539,0.418956634979468,6.8454265042638));
#7730=CARTESIAN_POINT('Ctrl Pts',(0.421037273012308,0.871132652579719,6.88747029453994));
#7731=CARTESIAN_POINT('Ctrl Pts',(-0.142342851291253,0.933831870869633,
6.92479402146672));
#7732=CARTESIAN_POINT('Ctrl Pts',(-0.575104466317865,0.724476767443434,
6.95741054274359));
#7733=CARTESIAN_POINT('Ctrl Pts',(-0.831597121038275,0.403171008458228,
6.98533606563364));
#7734=CARTESIAN_POINT('Ctrl Pts',(-0.922808904665035,0.00254068286457492,
7.01322724854536));
#7735=CARTESIAN_POINT('Ctrl Pts',(-0.831484359832733,-0.397369041930912,
7.04108128388358));
#7736=CARTESIAN_POINT('Ctrl Pts',(-0.576024516479058,-0.717622866946566,
7.06889539860548));
#7737=CARTESIAN_POINT('Ctrl Pts',(-0.207464718971416,-0.895095126308869,
7.09666685370961));
#7738=CARTESIAN_POINT('Ctrl Pts',(0.200869050822812,-0.894893573965507,
7.12439296344474));
#7739=CARTESIAN_POINT('Ctrl Pts',(0.568135301656786,-0.717941543510051,
7.15207107099507));
#7740=CARTESIAN_POINT('Ctrl Pts',(0.821742493579341,-0.399813712939291,
7.17969857736332));
#7741=CARTESIAN_POINT('Ctrl Pts',(0.912100647381109,-0.00372699171446918,
7.20727292857109));
#7742=CARTESIAN_POINT('Ctrl Pts',(0.821667160899362,0.391120281113409,7.23479162069698));
#7743=CARTESIAN_POINT('Ctrl Pts',(0.527798142032111,0.760706416566583,7.26682897888736));
#7744=CARTESIAN_POINT('Ctrl Pts',(0.00437094025093319,0.944184514671381,
7.30334225024583));
#7745=CARTESIAN_POINT('Ctrl Pts',(-0.583164611559206,0.738086874931468,
7.3442757526392));
#7746=CARTESIAN_POINT('Ctrl Pts',(-0.912546668924433,0.213026529714121,
7.38505770065783));
#7747=CARTESIAN_POINT('Ctrl Pts',(-0.843060529623956,-0.400706652853849,
7.42568118182012));
#7748=CARTESIAN_POINT('Ctrl Pts',(-0.407835437985135,-0.835237258109269,
7.46613873367218));
#7749=CARTESIAN_POINT('Ctrl Pts',(0.200737244244076,-0.903598468057941,
7.5064251969444));
#7750=CARTESIAN_POINT('Ctrl Pts',(0.71672352100227,-0.578479045751934,7.54653146106904));
#7751=CARTESIAN_POINT('Ctrl Pts',(0.849917343436364,-0.197265324952655,
7.57314919120958));
#7752=CARTESIAN_POINT('Ctrl Pts',(0.849943147209423,-0.00600671278230411,
7.58642685605973));
#7753=CARTESIAN_POINT('',(0.799999065628721,0.00692558823944227,5.30024010712383));
#7754=CARTESIAN_POINT('Origin',(0.8,-5.53479071733669E-17,5.4));
#7755=CARTESIAN_POINT('',(0.849943147209423,-0.00600671278230414,7.58642685605973));
#7756=CARTESIAN_POINT('Ctrl Pts',(0.799999065628721,0.00692558823944229,
5.30024010712383));
#7757=CARTESIAN_POINT('Ctrl Pts',(0.799974755250737,0.187114846749742,5.31274930893178));
#7758=CARTESIAN_POINT('Ctrl Pts',(0.674578200671659,0.546127076651831,5.33781512365923));
#7759=CARTESIAN_POINT('Ctrl Pts',(0.187998995393781,0.852903359039399,5.37564381521248));
#7760=CARTESIAN_POINT('Ctrl Pts',(-0.386721866921525,0.788448388841122,
5.41368605209984));
#7761=CARTESIAN_POINT('Ctrl Pts',(-0.7983994419892,0.377627224111744,5.45194644400096));
#7762=CARTESIAN_POINT('Ctrl Pts',(-0.864375113399524,-0.203617876612744,
5.49042055747836));
#7763=CARTESIAN_POINT('Ctrl Pts',(-0.552019639313923,-0.701812288635587,
5.52910737914477));
#7764=CARTESIAN_POINT('Ctrl Pts',(0.00615426428515267,-0.897757418326962,
5.56800374230524));
#7765=CARTESIAN_POINT('Ctrl Pts',(0.463089276607972,-0.737891299975203,
5.59986549204054));
#7766=CARTESIAN_POINT('Ctrl Pts',(0.706662565433678,-0.474149107376678,
5.62457829573124));
#7767=CARTESIAN_POINT('Ctrl Pts',(0.854347338563578,-0.169471123140589,
5.6478904398873));
#7768=CARTESIAN_POINT('Ctrl Pts',(0.854381411403854,0.269671075667267,5.67712918390586));
#7769=CARTESIAN_POINT('Ctrl Pts',(0.581578462406747,0.670744438556907,5.70943359497258));
#7770=CARTESIAN_POINT('Ctrl Pts',(0.189982000930166,0.858805851522918,5.73891161848027));
#7771=CARTESIAN_POINT('Ctrl Pts',(-0.201854620920769,0.859148371452269,
5.76552549972421));
#7772=CARTESIAN_POINT('Ctrl Pts',(-0.556170302204947,0.688486751453872,
5.79222147180784));
#7773=CARTESIAN_POINT('Ctrl Pts',(-0.802120584542054,0.380288702719923,
5.81899788702529));
#7774=CARTESIAN_POINT('Ctrl Pts',(-0.890321102734134,-0.0053444036833259,
5.84585301727138));
#7775=CARTESIAN_POINT('Ctrl Pts',(-0.816781798992104,-0.327577127496462,
5.86829638740099));
#7776=CARTESIAN_POINT('Ctrl Pts',(-0.678277859648778,-0.547664335405585,
5.88628859994389));
#7777=CARTESIAN_POINT('Ctrl Pts',(-0.494316135451619,-0.731945478665225,
5.90430550175064));
#7778=CARTESIAN_POINT('Ctrl Pts',(-0.194941007989142,-0.876310026230692,
5.92687230420244));
#7779=CARTESIAN_POINT('Ctrl Pts',(0.204945568353256,-0.876409485122255,
5.95402353339188));
#7780=CARTESIAN_POINT('Ctrl Pts',(0.566325487118899,-0.702556101088839,
5.98124373289334));
#7781=CARTESIAN_POINT('Ctrl Pts',(0.816751045229916,-0.388463305588866,
6.00853075028047));
#7782=CARTESIAN_POINT('Ctrl Pts',(0.917174982875959,0.0480250206861584,
6.03892142694837));
#7783=CARTESIAN_POINT('Ctrl Pts',(0.768829350780382,0.528866010776267,6.07244001895545));
#7784=CARTESIAN_POINT('Ctrl Pts',(0.338627495917749,0.872873034891815,6.10911095186911));
#7785=CARTESIAN_POINT('Ctrl Pts',(-0.212178222814091,0.914151313349766,
6.14588130840082));
#7786=CARTESIAN_POINT('Ctrl Pts',(-0.691759933067223,0.637451614256161,
6.18274515756461));
#7787=CARTESIAN_POINT('Ctrl Pts',(-0.932934482256533,0.137697594997002,
6.21969639210087));
#7788=CARTESIAN_POINT('Ctrl Pts',(-0.84730393945114,-0.435496308403701,
6.25827178793966));
#7789=CARTESIAN_POINT('Ctrl Pts',(-0.415273257958933,-0.868240176171726,
6.29847623644814));
#7790=CARTESIAN_POINT('Ctrl Pts',(0.146189896678077,-0.930950222024402,
6.33566388079779));
#7791=CARTESIAN_POINT('Ctrl Pts',(0.578787425776111,-0.722091726547751,
6.36825221458814));
#7792=CARTESIAN_POINT('Ctrl Pts',(0.835229259505866,-0.400278931762148,
6.3962159259868));
#7793=CARTESIAN_POINT('Ctrl Pts',(0.943177486850013,0.0688606453452641,
6.42887288667825));
#7794=CARTESIAN_POINT('Ctrl Pts',(0.756462512495389,0.604750444420971,6.46623690685835));
#7795=CARTESIAN_POINT('Ctrl Pts',(0.214509054547464,0.945343920852135,6.50831791566041));
#7796=CARTESIAN_POINT('Ctrl Pts',(-0.421585054233784,0.873670673138226,
6.55043539297339));
#7797=CARTESIAN_POINT('Ctrl Pts',(-0.874725713994987,0.420703846750279,
6.59257924943873));
#7798=CARTESIAN_POINT('Ctrl Pts',(-0.946491736933492,-0.216206220818672,
6.63473932973225));
#7799=CARTESIAN_POINT('Ctrl Pts',(-0.605472064685913,-0.758979181442101,
6.67690544450194));
#7800=CARTESIAN_POINT('Ctrl Pts',(-0.000509641250504898,-0.970641038681315,
6.71906739492544));
#7801=CARTESIAN_POINT('Ctrl Pts',(0.604236817182525,-0.758999928674301,
6.76121498571335));
#7802=CARTESIAN_POINT('Ctrl Pts',(0.944676427167983,-0.216670516455945,
6.80333805746961));
#7803=CARTESIAN_POINT('Ctrl Pts',(0.873719648783539,0.418956634979468,6.8454265042638));
#7804=CARTESIAN_POINT('Ctrl Pts',(0.421037273012308,0.871132652579719,6.88747029453994));
#7805=CARTESIAN_POINT('Ctrl Pts',(-0.142342851291253,0.933831870869633,
6.92479402146672));
#7806=CARTESIAN_POINT('Ctrl Pts',(-0.575104466317865,0.724476767443434,
6.95741054274359));
#7807=CARTESIAN_POINT('Ctrl Pts',(-0.831597121038275,0.403171008458228,
6.98533606563364));
#7808=CARTESIAN_POINT('Ctrl Pts',(-0.922808904665035,0.00254068286457492,
7.01322724854536));
#7809=CARTESIAN_POINT('Ctrl Pts',(-0.831484359832733,-0.397369041930912,
7.04108128388358));
#7810=CARTESIAN_POINT('Ctrl Pts',(-0.576024516479058,-0.717622866946566,
7.06889539860548));
#7811=CARTESIAN_POINT('Ctrl Pts',(-0.207464718971416,-0.895095126308869,
7.09666685370961));
#7812=CARTESIAN_POINT('Ctrl Pts',(0.200869050822812,-0.894893573965507,
7.12439296344474));
#7813=CARTESIAN_POINT('Ctrl Pts',(0.568135301656786,-0.717941543510051,
7.15207107099507));
#7814=CARTESIAN_POINT('Ctrl Pts',(0.821742493579341,-0.399813712939291,
7.17969857736332));
#7815=CARTESIAN_POINT('Ctrl Pts',(0.912100647381109,-0.00372699171446918,
7.20727292857109));
#7816=CARTESIAN_POINT('Ctrl Pts',(0.821667160899362,0.391120281113409,7.23479162069698));
#7817=CARTESIAN_POINT('Ctrl Pts',(0.527798142032111,0.760706416566583,7.26682897888736));
#7818=CARTESIAN_POINT('Ctrl Pts',(0.00437094025093319,0.944184514671381,
7.30334225024583));
#7819=CARTESIAN_POINT('Ctrl Pts',(-0.583164611559206,0.738086874931468,
7.3442757526392));
#7820=CARTESIAN_POINT('Ctrl Pts',(-0.912546668924433,0.213026529714121,
7.38505770065783));
#7821=CARTESIAN_POINT('Ctrl Pts',(-0.843060529623956,-0.400706652853849,
7.42568118182012));
#7822=CARTESIAN_POINT('Ctrl Pts',(-0.407835437985135,-0.835237258109269,
7.46613873367218));
#7823=CARTESIAN_POINT('Ctrl Pts',(0.200737244244076,-0.903598468057941,
7.5064251969444));
#7824=CARTESIAN_POINT('Ctrl Pts',(0.71672352100227,-0.578479045751934,7.54653146106904));
#7825=CARTESIAN_POINT('Ctrl Pts',(0.849917343436364,-0.197265324952655,
7.57314919120958));
#7826=CARTESIAN_POINT('Ctrl Pts',(0.849943147209423,-0.00600671278230411,
7.58642685605973));
#7827=CARTESIAN_POINT('Origin',(0.799999999999999,-1.22124532708767E-15,
7.5));
#7828=CARTESIAN_POINT('Origin',(0.799999999999999,-1.22124532708767E-15,
7.5));
#7829=CARTESIAN_POINT('Origin',(0.8,-5.53479071733669E-17,5.4));
#7830=CARTESIAN_POINT('',(0.,0.,0.));
#7831=CARTESIAN_POINT('Origin',(0.,0.,7.2));
#7832=CARTESIAN_POINT('',(-0.6,-7.34788079488412E-17,7.6));
#7833=CARTESIAN_POINT('Origin',(0.,0.,7.6));
#7834=CARTESIAN_POINT('',(-0.6,-7.34788079488412E-17,7.2));
#7835=CARTESIAN_POINT('',(-0.6,-7.34788079488412E-17,7.2));
#7836=CARTESIAN_POINT('Origin',(0.,0.,7.2));
#7837=CARTESIAN_POINT('Origin',(0.,0.,7.2));
#7838=CARTESIAN_POINT('Origin',(0.,0.,7.6));
#7839=CARTESIAN_POINT('',(-1.2,-1.46957615897682E-16,8.));
#7840=CARTESIAN_POINT('Origin',(0.,0.,8.));
#7841=CARTESIAN_POINT('',(-1.2,-1.46957615897682E-16,7.6));
#7842=CARTESIAN_POINT('',(-1.2,-1.46957615897682E-16,7.6));
#7843=CARTESIAN_POINT('Origin',(0.,0.,7.6));
#7844=CARTESIAN_POINT('Origin',(0.,0.,8.));
#7845=CARTESIAN_POINT('Origin',(0.,0.,7.6));
#7846=CARTESIAN_POINT('',(0.,0.,0.));
#7847=CARTESIAN_POINT('Origin',(0.,0.,8.));
#7848=CARTESIAN_POINT('',(-0.4,-4.89858719658941E-17,11.));
#7849=CARTESIAN_POINT('Origin',(0.,0.,11.));
#7850=CARTESIAN_POINT('',(-0.4,-4.89858719658941E-17,8.));
#7851=CARTESIAN_POINT('',(-0.4,-4.89858719658941E-17,8.));
#7852=CARTESIAN_POINT('Origin',(0.,0.,8.));
#7853=CARTESIAN_POINT('Origin',(0.,0.,11.));
#7854=CARTESIAN_POINT('Origin',(0.,0.,8.));
#7855=CARTESIAN_POINT('',(0.,0.,0.));
#7856=CARTESIAN_POINT('Origin',(0.,0.39,11.));
#7857=CARTESIAN_POINT('',(-0.088881944173156,0.39,10.8609856122554));
#7858=CARTESIAN_POINT('',(-0.088881944173156,0.39,11.1390143877446));
#7859=CARTESIAN_POINT('',(-0.088881944173156,0.39,10.5));
#7860=CARTESIAN_POINT('',(-0.165,0.39,11.));
#7861=CARTESIAN_POINT('Origin',(0.,0.39,11.));
#7862=CARTESIAN_POINT('Origin',(0.,0.39,11.));
#7863=CARTESIAN_POINT('Origin',(0.,0.39,11.));
#7864=CARTESIAN_POINT('',(0.088881944173156,0.39,10.8609856122554));
#7865=CARTESIAN_POINT('Ctrl Pts',(0.088881944173156,0.39,10.8609856122554));
#7866=CARTESIAN_POINT('Ctrl Pts',(0.0808964434200154,0.391819914954193,
10.8558799045395));
#7867=CARTESIAN_POINT('Ctrl Pts',(0.072364333302368,0.393502517883282,10.8514036081398));
#7868=CARTESIAN_POINT('Ctrl Pts',(0.0431949313468624,0.398191715532106,
10.8392437758303));
#7869=CARTESIAN_POINT('Ctrl Pts',(0.0209808024963256,0.4,10.835));
#7870=CARTESIAN_POINT('Ctrl Pts',(-0.0209808024963256,0.4,10.835));
#7871=CARTESIAN_POINT('Ctrl Pts',(-0.0431949313468624,0.398191715532106,
10.8392437758303));
#7872=CARTESIAN_POINT('Ctrl Pts',(-0.072364333302368,0.393502517883282,
10.8514036081398));
#7873=CARTESIAN_POINT('Ctrl Pts',(-0.0808964434200154,0.391819914954193,
10.8558799045395));
#7874=CARTESIAN_POINT('Ctrl Pts',(-0.088881944173156,0.39,10.8609856122554));
#7875=CARTESIAN_POINT('',(0.088881944173156,0.39,11.1390143877446));
#7876=CARTESIAN_POINT('Origin',(0.,0.39,11.));
#7877=CARTESIAN_POINT('Ctrl Pts',(-0.088881944173156,0.39,11.1390143877446));
#7878=CARTESIAN_POINT('Ctrl Pts',(-0.0808964434200154,0.391819914954193,
11.1441200954605));
#7879=CARTESIAN_POINT('Ctrl Pts',(-0.072364333302368,0.393502517883282,
11.1485963918602));
#7880=CARTESIAN_POINT('Ctrl Pts',(-0.0431949313468623,0.398191715532106,
11.1607562241697));
#7881=CARTESIAN_POINT('Ctrl Pts',(-0.0209808024963255,0.4,11.165));
#7882=CARTESIAN_POINT('Ctrl Pts',(0.0209808024963256,0.4,11.165));
#7883=CARTESIAN_POINT('Ctrl Pts',(0.0431949313468623,0.398191715532106,
11.1607562241697));
#7884=CARTESIAN_POINT('Ctrl Pts',(0.072364333302368,0.393502517883282,11.1485963918602));
#7885=CARTESIAN_POINT('Ctrl Pts',(0.0808964434200153,0.391819914954193,
11.1441200954605));
#7886=CARTESIAN_POINT('Ctrl Pts',(0.088881944173156,0.39,11.1390143877446));
#7887=CARTESIAN_POINT('',(-0.165,1.49089738077441,11.));
#7888=CARTESIAN_POINT('',(-0.165,0.39,11.));
#7889=CARTESIAN_POINT('Ctrl Pts',(-0.165,1.49089738077441,11.));
#7890=CARTESIAN_POINT('Ctrl Pts',(-0.165,1.49089738077441,10.979264160895));
#7891=CARTESIAN_POINT('Ctrl Pts',(-0.160852499025073,1.49137458218466,10.9571577290991));
#7892=CARTESIAN_POINT('Ctrl Pts',(-0.144008447160944,1.49309518705251,10.916510155069));
#7893=CARTESIAN_POINT('Ctrl Pts',(-0.131312810193433,1.49431341615515,10.8979675724019));
#7894=CARTESIAN_POINT('Ctrl Pts',(-0.102032500700889,1.49659781052539,10.8686872629093));
#7895=CARTESIAN_POINT('Ctrl Pts',(-0.0834898860986569,1.49781281581157,
10.8559915687804));
#7896=CARTESIAN_POINT('Ctrl Pts',(-0.042842204593242,1.49952603771524,10.8391474746158));
#7897=CARTESIAN_POINT('Ctrl Pts',(-0.0207357355648686,1.5,10.835));
#7898=CARTESIAN_POINT('Ctrl Pts',(0.0207357355648686,1.5,10.835));
#7899=CARTESIAN_POINT('Ctrl Pts',(0.0428422045932419,1.49952603771524,10.8391474746158));
#7900=CARTESIAN_POINT('Ctrl Pts',(0.0834898860986569,1.49781281581157,10.8559915687804));
#7901=CARTESIAN_POINT('Ctrl Pts',(0.102032500700889,1.49659781052539,10.8686872629093));
#7902=CARTESIAN_POINT('Ctrl Pts',(0.131312810193433,1.49431341615515,10.8979675724019));
#7903=CARTESIAN_POINT('Ctrl Pts',(0.144008447160944,1.49309518705251,10.916510155069));
#7904=CARTESIAN_POINT('Ctrl Pts',(0.160852499025073,1.49137458218466,10.9571577290991));
#7905=CARTESIAN_POINT('Ctrl Pts',(0.165,1.49089738077441,10.979264160895));
#7906=CARTESIAN_POINT('Ctrl Pts',(0.165,1.49089738077441,11.020735839105));
#7907=CARTESIAN_POINT('Ctrl Pts',(0.160852499025073,1.49137458218466,11.0428422709009));
#7908=CARTESIAN_POINT('Ctrl Pts',(0.144008447160944,1.49309518705251,11.083489844931));
#7909=CARTESIAN_POINT('Ctrl Pts',(0.131312810193433,1.49431341615515,11.1020324275981));
#7910=CARTESIAN_POINT('Ctrl Pts',(0.102032500700889,1.49659781052539,11.1313127370907));
#7911=CARTESIAN_POINT('Ctrl Pts',(0.0834898860986569,1.49781281581157,11.1440084312196));
#7912=CARTESIAN_POINT('Ctrl Pts',(0.042842204593242,1.49952603771524,11.1608525253842));
#7913=CARTESIAN_POINT('Ctrl Pts',(0.0207357355648686,1.5,11.165));
#7914=CARTESIAN_POINT('Ctrl Pts',(-0.0207357355648686,1.5,11.165));
#7915=CARTESIAN_POINT('Ctrl Pts',(-0.0428422045932419,1.49952603771524,
11.1608525253842));
#7916=CARTESIAN_POINT('Ctrl Pts',(-0.0834898860986569,1.49781281581157,
11.1440084312196));
#7917=CARTESIAN_POINT('Ctrl Pts',(-0.102032500700889,1.49659781052539,11.1313127370907));
#7918=CARTESIAN_POINT('Ctrl Pts',(-0.131312810193433,1.49431341615515,11.1020324275981));
#7919=CARTESIAN_POINT('Ctrl Pts',(-0.144008447160944,1.49309518705251,11.083489844931));
#7920=CARTESIAN_POINT('Ctrl Pts',(-0.160852499025073,1.49137458218466,11.0428422709009));
#7921=CARTESIAN_POINT('Ctrl Pts',(-0.165,1.49089738077441,11.020735839105));
#7922=CARTESIAN_POINT('Ctrl Pts',(-0.165,1.49089738077441,11.));
#7923=CARTESIAN_POINT('Origin',(0.,0.39,11.));
#7924=CARTESIAN_POINT('',(0.088881944173156,0.39,10.5));
#7925=CARTESIAN_POINT('Origin',(0.,0.,10.5));
#7926=CARTESIAN_POINT('',(-0.4,-4.89858719658941E-17,11.5));
#7927=CARTESIAN_POINT('Origin',(0.,0.,11.5));
#7928=CARTESIAN_POINT('',(-0.4,-4.89858719658941E-17,10.5));
#7929=CARTESIAN_POINT('',(-0.4,-4.89858719658941E-17,10.5));
#7930=CARTESIAN_POINT('Origin',(0.,0.,10.5));
#7931=CARTESIAN_POINT('Origin',(0.,0.,10.5));
#7932=CARTESIAN_POINT('',(-1.5,-1.83697019872103E-16,11.5));
#7933=CARTESIAN_POINT('Origin',(0.,0.,11.5));
#7934=CARTESIAN_POINT('',(-1.5,-1.83697019872103E-16,10.5));
#7935=CARTESIAN_POINT('',(-1.5,-1.83697019872103E-16,10.5));
#7936=CARTESIAN_POINT('Origin',(0.,0.,10.5));
#7937=CARTESIAN_POINT('Origin',(0.,0.,11.5));
#7938=CARTESIAN_POINT('Origin',(0.,0.,10.5));
#7939=CARTESIAN_POINT('',(0.,0.,0.));
#7940=CARTESIAN_POINT('Origin',(-4.,4.5,-0.6));
#7941=CARTESIAN_POINT('',(-4.,4.5,-0.6));
#7942=CARTESIAN_POINT('',(-6.,4.5,-0.6));
#7943=CARTESIAN_POINT('',(-4.,4.5,-0.6));
#7944=CARTESIAN_POINT('',(-6.,4.5,0.));
#7945=CARTESIAN_POINT('',(-6.,4.5,-0.6));
#7946=CARTESIAN_POINT('',(-4.,4.5,0.));
#7947=CARTESIAN_POINT('',(-4.,4.5,0.));
#7948=CARTESIAN_POINT('',(-4.,4.5,-0.6));
#7949=CARTESIAN_POINT('Origin',(-4.,-4.5,-0.6));
#7950=CARTESIAN_POINT('',(-4.,-4.5,-0.6));
#7951=CARTESIAN_POINT('',(-4.,-4.5,-0.6));
#7952=CARTESIAN_POINT('',(-4.,-4.5,0.));
#7953=CARTESIAN_POINT('',(-4.,-4.5,0.));
#7954=CARTESIAN_POINT('',(-4.,-4.5,-0.6));
#7955=CARTESIAN_POINT('Origin',(-6.,-4.5,-0.6));
#7956=CARTESIAN_POINT('',(-6.,-4.5,-0.6));
#7957=CARTESIAN_POINT('',(-6.,-4.5,-0.6));
#7958=CARTESIAN_POINT('',(-6.,-4.5,0.));
#7959=CARTESIAN_POINT('',(-6.,-4.5,0.));
#7960=CARTESIAN_POINT('',(-6.,-4.5,-0.6));
#7961=CARTESIAN_POINT('Origin',(-6.,4.5,-0.6));
#7962=CARTESIAN_POINT('',(-6.,4.5,-0.6));
#7963=CARTESIAN_POINT('',(-6.,4.5,0.));
#7964=CARTESIAN_POINT('Origin',(-5.,0.,0.));
#7965=CARTESIAN_POINT('Origin',(-5.,0.,-0.6));
#7966=CARTESIAN_POINT('',(0.,0.,0.));
#7967=CARTESIAN_POINT('Origin',(6.,4.5,-0.6));
#7968=CARTESIAN_POINT('',(6.,4.5,-0.6));
#7969=CARTESIAN_POINT('',(4.,4.5,-0.6));
#7970=CARTESIAN_POINT('',(6.,4.5,-0.6));
#7971=CARTESIAN_POINT('',(4.,4.5,0.));
#7972=CARTESIAN_POINT('',(4.,4.5,-0.6));
#7973=CARTESIAN_POINT('',(6.,4.5,0.));
#7974=CARTESIAN_POINT('',(6.,4.5,0.));
#7975=CARTESIAN_POINT('',(6.,4.5,-0.6));
#7976=CARTESIAN_POINT('Origin',(6.,-4.5,-0.6));
#7977=CARTESIAN_POINT('',(6.,-4.5,-0.6));
#7978=CARTESIAN_POINT('',(6.,-4.5,-0.6));
#7979=CARTESIAN_POINT('',(6.,-4.5,0.));
#7980=CARTESIAN_POINT('',(6.,-4.5,0.));
#7981=CARTESIAN_POINT('',(6.,-4.5,-0.6));
#7982=CARTESIAN_POINT('Origin',(4.,-4.5,-0.6));
#7983=CARTESIAN_POINT('',(4.,-4.5,-0.6));
#7984=CARTESIAN_POINT('',(4.,-4.5,-0.6));
#7985=CARTESIAN_POINT('',(4.,-4.5,0.));
#7986=CARTESIAN_POINT('',(4.,-4.5,0.));
#7987=CARTESIAN_POINT('',(4.,-4.5,-0.6));
#7988=CARTESIAN_POINT('Origin',(4.,4.5,-0.6));
#7989=CARTESIAN_POINT('',(4.,4.5,-0.6));
#7990=CARTESIAN_POINT('',(4.,4.5,0.));
#7991=CARTESIAN_POINT('Origin',(5.,0.,0.));
#7992=CARTESIAN_POINT('Origin',(5.,0.,-0.6));
#7993=CARTESIAN_POINT('',(0.,0.,0.));
#7994=CARTESIAN_POINT('Origin',(0.3,0.4,0.));
#7995=CARTESIAN_POINT('',(-0.3,0.4,-3.67394039744206E-17));
#7996=CARTESIAN_POINT('Origin',(0.,0.4,0.));
#7997=CARTESIAN_POINT('Origin',(0.,0.375,0.));
#7998=CARTESIAN_POINT('',(-0.35,0.35,-4.28626379701573E-17));
#7999=CARTESIAN_POINT('Origin',(0.,0.35,0.));
#8000=CARTESIAN_POINT('',(-0.325,0.375,-3.9801020972289E-17));
#8001=CARTESIAN_POINT('Origin',(0.,0.19,0.));
#8002=CARTESIAN_POINT('',(-0.35,0.03,-4.28626379701574E-17));
#8003=CARTESIAN_POINT('Origin',(0.,0.03,0.));
#8004=CARTESIAN_POINT('',(-0.35,0.19,-4.28626379701574E-17));
#8005=CARTESIAN_POINT('Origin',(0.,0.0149999999999999,0.));
#8006=CARTESIAN_POINT('',(-0.32,-3.29597460435593E-17,-3.91886975727153E-17));
#8007=CARTESIAN_POINT('Origin',(0.,0.,0.));
#8008=CARTESIAN_POINT('',(-0.335,0.0149999999999999,-4.10256677714363E-17));
#8009=CARTESIAN_POINT('Origin',(0.22,0.,0.));
#8010=CARTESIAN_POINT('',(-0.22,-6.93889390390723E-18,-2.69422295812418E-17));
#8011=CARTESIAN_POINT('Origin',(0.,0.,0.));
#8012=CARTESIAN_POINT('Origin',(0.,-0.02,0.));
#8013=CARTESIAN_POINT('',(-0.1954,-0.0492,2.39295984553393E-17));
#8014=CARTESIAN_POINT('Origin',(0.,-0.0492,0.));
#8015=CARTESIAN_POINT('',(-0.21,-0.02,-2.57175827820944E-17));
#8016=CARTESIAN_POINT('Origin',(0.,-0.8,0.));
#8017=CARTESIAN_POINT('',(-0.1954,-1.5646,2.39295984553393E-17));
#8018=CARTESIAN_POINT('Origin',(0.,-1.5646,0.));
#8019=CARTESIAN_POINT('',(-0.1954,-0.8,-2.39295984553393E-17));
#8020=CARTESIAN_POINT('Origin',(0.,-1.58,0.));
#8021=CARTESIAN_POINT('',(-0.16,-1.6,-1.95943487863577E-17));
#8022=CARTESIAN_POINT('Origin',(0.,-1.6,0.));
#8023=CARTESIAN_POINT('',(-0.18,-1.58,-2.20436423846524E-17));
#8024=CARTESIAN_POINT('Origin',(0.,-1.6,0.));
#8025=CARTESIAN_POINT('Origin',(0.0866025403784439,-0.4,-0.15));
#8026=CARTESIAN_POINT('',(0.173205080756888,-0.4,0.));
#8027=CARTESIAN_POINT('',(0.0866025403784439,-0.4,-0.15));
#8028=CARTESIAN_POINT('',(0.173205080756888,-0.4,0.));
#8029=CARTESIAN_POINT('',(0.0866025403784439,-0.64,-0.15));
#8030=CARTESIAN_POINT('',(0.0866025403784439,-0.4,-0.15));
#8031=CARTESIAN_POINT('',(0.173205080756888,-0.64,0.));
#8032=CARTESIAN_POINT('',(0.173205080756888,-0.64,0.));
#8033=CARTESIAN_POINT('',(0.173205080756888,-0.4,0.));
#8034=CARTESIAN_POINT('Origin',(-0.0866025403784438,-0.4,-0.15));
#8035=CARTESIAN_POINT('',(-0.0866025403784438,-0.4,-0.15));
#8036=CARTESIAN_POINT('',(0.0866025403784439,-0.4,-0.15));
#8037=CARTESIAN_POINT('',(-0.0866025403784438,-0.64,-0.15));
#8038=CARTESIAN_POINT('',(-0.0866025403784438,-0.4,-0.15));
#8039=CARTESIAN_POINT('',(0.0866025403784439,-0.64,-0.15));
#8040=CARTESIAN_POINT('Origin',(-0.173205080756888,-0.4,-2.77555756156289E-17));
#8041=CARTESIAN_POINT('',(-0.173205080756888,-0.4,-2.12115047744981E-17));
#8042=CARTESIAN_POINT('',(-0.0866025403784438,-0.4,-0.15));
#8043=CARTESIAN_POINT('',(-0.173205080756888,-0.64,-2.77555756156289E-17));
#8044=CARTESIAN_POINT('',(-0.173205080756888,-0.4,-2.12115047744981E-17));
#8045=CARTESIAN_POINT('',(-0.0866025403784438,-0.64,-0.15));
#8046=CARTESIAN_POINT('Origin',(-0.0866025403784439,-0.4,0.15));
#8047=CARTESIAN_POINT('',(-0.0866025403784439,-0.4,0.15));
#8048=CARTESIAN_POINT('',(-0.173205080756888,-0.4,-2.12115047744981E-17));
#8049=CARTESIAN_POINT('',(-0.0866025403784439,-0.64,0.15));
#8050=CARTESIAN_POINT('',(-0.0866025403784439,-0.4,0.15));
#8051=CARTESIAN_POINT('',(-0.173205080756888,-0.64,-2.12115047744981E-17));
#8052=CARTESIAN_POINT('Origin',(0.0866025403784439,-0.4,0.15));
#8053=CARTESIAN_POINT('',(0.0866025403784439,-0.4,0.15));
#8054=CARTESIAN_POINT('',(-0.0866025403784439,-0.4,0.15));
#8055=CARTESIAN_POINT('',(0.0866025403784439,-0.64,0.15));
#8056=CARTESIAN_POINT('',(0.0866025403784439,-0.4,0.15));
#8057=CARTESIAN_POINT('',(-0.0866025403784439,-0.64,0.15));
#8058=CARTESIAN_POINT('Origin',(0.173205080756888,-0.4,0.));
#8059=CARTESIAN_POINT('',(0.0866025403784439,-0.4,0.15));
#8060=CARTESIAN_POINT('',(0.0866025403784439,-0.64,0.15));
#8061=CARTESIAN_POINT('Origin',(0.,-0.4,-2.77555756156289E-17));
#8062=CARTESIAN_POINT('Origin',(0.,-0.64,-2.77555756156289E-17));
#8063=CARTESIAN_POINT('',(0.,0.,0.));
#8064=CARTESIAN_POINT('Origin',(0.,-0.4,0.));
#8065=CARTESIAN_POINT('',(1.01036297108185,-0.4,0.));
#8066=CARTESIAN_POINT('',(0.505181485540923,-0.4,0.875));
#8067=CARTESIAN_POINT('',(0.505181485540923,-0.4,0.875));
#8068=CARTESIAN_POINT('',(-0.505181485540923,-0.4,0.875));
#8069=CARTESIAN_POINT('',(-0.505181485540923,-0.4,0.875));
#8070=CARTESIAN_POINT('',(-1.01036297108185,-0.4,-1.23733777851239E-16));
#8071=CARTESIAN_POINT('',(-1.01036297108185,-0.4,-1.23733777851239E-16));
#8072=CARTESIAN_POINT('',(-0.505181485540922,-0.4,-0.875));
#8073=CARTESIAN_POINT('',(-0.505181485540922,-0.4,-0.875));
#8074=CARTESIAN_POINT('',(0.505181485540923,-0.4,-0.875));
#8075=CARTESIAN_POINT('',(0.505181485540923,-0.4,-0.875));
#8076=CARTESIAN_POINT('',(1.01036297108185,-0.4,0.));
#8077=CARTESIAN_POINT('',(-0.685,-0.4,-8.38883057415937E-17));
#8078=CARTESIAN_POINT('Origin',(0.,-0.4,0.));
#8079=CARTESIAN_POINT('Origin',(0.,0.4,0.));
#8080=CARTESIAN_POINT('',(0.505181485540923,0.4,0.875));
#8081=CARTESIAN_POINT('',(1.01036297108185,0.4,0.));
#8082=CARTESIAN_POINT('',(0.505181485540923,0.4,0.875));
#8083=CARTESIAN_POINT('',(0.505181485540923,0.4,-0.875));
#8084=CARTESIAN_POINT('',(1.01036297108185,0.4,0.));
#8085=CARTESIAN_POINT('',(-0.505181485540922,0.4,-0.875));
#8086=CARTESIAN_POINT('',(0.505181485540923,0.4,-0.875));
#8087=CARTESIAN_POINT('',(-1.01036297108185,0.4,-1.23733777851239E-16));
#8088=CARTESIAN_POINT('',(-0.505181485540922,0.4,-0.875));
#8089=CARTESIAN_POINT('',(-0.505181485540923,0.4,0.875));
#8090=CARTESIAN_POINT('',(-1.01036297108185,0.4,-1.23733777851239E-16));
#8091=CARTESIAN_POINT('',(-0.505181485540923,0.4,0.875));
#8092=CARTESIAN_POINT('',(-0.685,0.4,8.38883057415937E-17));
#8093=CARTESIAN_POINT('Origin',(0.,0.4,0.));
#8094=CARTESIAN_POINT('Origin',(-0.505181485540923,0.,0.875));
#8095=CARTESIAN_POINT('',(0.505181485540923,0.,0.875));
#8096=CARTESIAN_POINT('',(-0.505181485540923,0.,0.875));
#8097=CARTESIAN_POINT('Origin',(-1.01036297108185,0.,-1.23733777851239E-16));
#8098=CARTESIAN_POINT('',(-1.01036297108185,0.,-1.23733777851239E-16));
#8099=CARTESIAN_POINT('Origin',(-0.505181485540922,0.,-0.875));
#8100=CARTESIAN_POINT('',(-0.505181485540922,0.,-0.875));
#8101=CARTESIAN_POINT('Origin',(0.505181485540923,0.,-0.875));
#8102=CARTESIAN_POINT('',(0.505181485540923,0.,-0.875));
#8103=CARTESIAN_POINT('Origin',(1.01036297108185,0.,0.));
#8104=CARTESIAN_POINT('',(1.01036297108185,0.,0.));
#8105=CARTESIAN_POINT('Origin',(0.505181485540923,0.,0.875));
#8106=CARTESIAN_POINT('Origin',(0.,0.,0.));
#8107=CARTESIAN_POINT('',(-0.685,1.82,-8.38883057415937E-17));
#8108=CARTESIAN_POINT('',(-0.685,0.,-8.38883057415937E-17));
#8109=CARTESIAN_POINT('Origin',(0.,1.82,0.));
#8110=CARTESIAN_POINT('Origin',(0.605,1.9,0.));
#8111=CARTESIAN_POINT('',(-0.605,1.9,-7.40911313484149E-17));
#8112=CARTESIAN_POINT('Origin',(0.,1.9,0.));
#8113=CARTESIAN_POINT('',(-0.46,1.9,-5.63337527607782E-17));
#8114=CARTESIAN_POINT('Origin',(0.,1.9,0.));
#8115=CARTESIAN_POINT('Origin',(0.,1.86,0.));
#8116=CARTESIAN_POINT('',(-0.645,1.86,-7.89897185450043E-17));
#8117=CARTESIAN_POINT('Origin',(0.,0.,0.));
#8118=CARTESIAN_POINT('',(-0.685,-1.82,-8.38883057415937E-17));
#8119=CARTESIAN_POINT('Origin',(0.,-1.82,0.));
#8120=CARTESIAN_POINT('',(-0.685,0.,-8.38883057415937E-17));
#8121=CARTESIAN_POINT('Origin',(0.,-1.86,0.));
#8122=CARTESIAN_POINT('',(-0.605,-1.9,-7.40911313484149E-17));
#8123=CARTESIAN_POINT('Origin',(0.,-1.9,0.));
#8124=CARTESIAN_POINT('',(-0.645,-1.86,-7.89897185450043E-17));
#8125=CARTESIAN_POINT('Origin',(0.46,-1.9,0.));
#8126=CARTESIAN_POINT('',(-0.46,-1.9,-5.63337527607782E-17));
#8127=CARTESIAN_POINT('Origin',(0.,-1.9,0.));
#8128=CARTESIAN_POINT('Origin',(0.,0.,0.));
#8129=CARTESIAN_POINT('',(-0.46,0.,-5.63337527607782E-17));
#8130=CARTESIAN_POINT('',(0.,0.,0.));
#8131=CARTESIAN_POINT('Origin',(0.375,0.5,0.));
#8132=CARTESIAN_POINT('',(-0.375,0.5,-4.59242549680257E-17));
#8133=CARTESIAN_POINT('Origin',(0.,0.5,0.));
#8134=CARTESIAN_POINT('Origin',(0.,0.475,0.));
#8135=CARTESIAN_POINT('',(-0.425,0.45,-5.20474889637625E-17));
#8136=CARTESIAN_POINT('Origin',(0.,0.45,0.));
#8137=CARTESIAN_POINT('',(-0.4,0.475,-4.89858719658941E-17));
#8138=CARTESIAN_POINT('Origin',(0.,0.24,0.));
#8139=CARTESIAN_POINT('',(-0.425,0.0299999999999998,-5.20474889637625E-17));
#8140=CARTESIAN_POINT('Origin',(0.,0.0299999999999998,0.));
#8141=CARTESIAN_POINT('',(-0.425,0.24,-5.20474889637625E-17));
#8142=CARTESIAN_POINT('Origin',(0.,0.0150000000000001,0.));
#8143=CARTESIAN_POINT('',(-0.395,4.85722573273506E-17,-4.83735485663204E-17));
#8144=CARTESIAN_POINT('Origin',(0.,0.,0.));
#8145=CARTESIAN_POINT('',(-0.41,0.0150000000000001,-5.02105187650415E-17));
#8146=CARTESIAN_POINT('Origin',(0.27,0.,0.));
#8147=CARTESIAN_POINT('',(-0.27,0.,-3.30654635769785E-17));
#8148=CARTESIAN_POINT('Origin',(0.,0.,0.));
#8149=CARTESIAN_POINT('Origin',(0.,-0.02,0.));
#8150=CARTESIAN_POINT('',(-0.24505,-0.0498999999999999,3.00099698131059E-17));
#8151=CARTESIAN_POINT('Origin',(0.,-0.0498999999999999,0.));
#8152=CARTESIAN_POINT('',(-0.26,-0.02,-3.18408167778312E-17));
#8153=CARTESIAN_POINT('Origin',(0.,-0.995,0.));
#8154=CARTESIAN_POINT('',(-0.24505,-1.95495,3.00099698131059E-17));
#8155=CARTESIAN_POINT('Origin',(0.,-1.95495,0.));
#8156=CARTESIAN_POINT('',(-0.24505,-0.995,-3.00099698131059E-17));
#8157=CARTESIAN_POINT('Origin',(0.,-1.975,0.));
#8158=CARTESIAN_POINT('',(-0.2,-2.,-2.44929359829471E-17));
#8159=CARTESIAN_POINT('Origin',(0.,-2.,0.));
#8160=CARTESIAN_POINT('',(-0.225,-1.975,-2.75545529808154E-17));
#8161=CARTESIAN_POINT('Origin',(0.,-2.,0.));
#8162=CARTESIAN_POINT('Origin',(0.115470053837925,-0.5,-0.2));
#8163=CARTESIAN_POINT('',(0.23094010767585,-0.5,0.));
#8164=CARTESIAN_POINT('',(0.115470053837925,-0.5,-0.2));
#8165=CARTESIAN_POINT('',(0.23094010767585,-0.5,0.));
#8166=CARTESIAN_POINT('',(0.115470053837925,-0.8,-0.2));
#8167=CARTESIAN_POINT('',(0.115470053837925,-0.5,-0.2));
#8168=CARTESIAN_POINT('',(0.23094010767585,-0.8,0.));
#8169=CARTESIAN_POINT('',(0.23094010767585,-0.8,0.));
#8170=CARTESIAN_POINT('',(0.23094010767585,-0.5,0.));
#8171=CARTESIAN_POINT('Origin',(-0.115470053837925,-0.5,-0.2));
#8172=CARTESIAN_POINT('',(-0.115470053837925,-0.5,-0.2));
#8173=CARTESIAN_POINT('',(0.115470053837925,-0.5,-0.2));
#8174=CARTESIAN_POINT('',(-0.115470053837925,-0.8,-0.2));
#8175=CARTESIAN_POINT('',(-0.115470053837925,-0.5,-0.2));
#8176=CARTESIAN_POINT('',(0.115470053837925,-0.8,-0.2));
#8177=CARTESIAN_POINT('Origin',(-0.23094010767585,-0.5,-2.77555756156289E-17));
#8178=CARTESIAN_POINT('',(-0.23094010767585,-0.5,-2.82820063659975E-17));
#8179=CARTESIAN_POINT('',(-0.115470053837925,-0.5,-0.2));
#8180=CARTESIAN_POINT('',(-0.23094010767585,-0.8,-2.77555756156289E-17));
#8181=CARTESIAN_POINT('',(-0.23094010767585,-0.5,-2.82820063659975E-17));
#8182=CARTESIAN_POINT('',(-0.115470053837925,-0.8,-0.2));
#8183=CARTESIAN_POINT('Origin',(-0.115470053837925,-0.5,0.2));
#8184=CARTESIAN_POINT('',(-0.115470053837925,-0.5,0.2));
#8185=CARTESIAN_POINT('',(-0.23094010767585,-0.5,-2.82820063659975E-17));
#8186=CARTESIAN_POINT('',(-0.115470053837925,-0.8,0.2));
#8187=CARTESIAN_POINT('',(-0.115470053837925,-0.5,0.2));
#8188=CARTESIAN_POINT('',(-0.23094010767585,-0.8,-2.82820063659975E-17));
#8189=CARTESIAN_POINT('Origin',(0.115470053837925,-0.5,0.2));
#8190=CARTESIAN_POINT('',(0.115470053837925,-0.5,0.2));
#8191=CARTESIAN_POINT('',(-0.115470053837925,-0.5,0.2));
#8192=CARTESIAN_POINT('',(0.115470053837925,-0.8,0.2));
#8193=CARTESIAN_POINT('',(0.115470053837925,-0.5,0.2));
#8194=CARTESIAN_POINT('',(-0.115470053837925,-0.8,0.2));
#8195=CARTESIAN_POINT('Origin',(0.23094010767585,-0.5,0.));
#8196=CARTESIAN_POINT('',(0.115470053837925,-0.5,0.2));
#8197=CARTESIAN_POINT('',(0.115470053837925,-0.8,0.2));
#8198=CARTESIAN_POINT('Origin',(0.,-0.5,0.));
#8199=CARTESIAN_POINT('Origin',(0.,-0.8,0.));
#8200=CARTESIAN_POINT('',(0.,0.,0.));
#8201=CARTESIAN_POINT('Origin',(0.,0.,0.));
#8202=CARTESIAN_POINT('',(-0.42,0.16,5.14351655641888E-17));
#8203=CARTESIAN_POINT('Origin',(0.,0.16,0.));
#8204=CARTESIAN_POINT('',(-0.42,0.,5.14351655641888E-17));
#8205=CARTESIAN_POINT('',(-0.42,0.,5.14351655641888E-17));
#8206=CARTESIAN_POINT('Origin',(0.,0.,0.));
#8207=CARTESIAN_POINT('Origin',(0.,0.,0.));
#8208=CARTESIAN_POINT('',(-0.8,0.16,9.79717439317883E-17));
#8209=CARTESIAN_POINT('Origin',(0.,0.16,0.));
#8210=CARTESIAN_POINT('',(-0.8,0.,9.79717439317883E-17));
#8211=CARTESIAN_POINT('',(-0.8,0.,9.79717439317883E-17));
#8212=CARTESIAN_POINT('Origin',(0.,0.,0.));
#8213=CARTESIAN_POINT('Origin',(0.,0.16,0.));
#8214=CARTESIAN_POINT('Origin',(0.,0.,0.));
#8215=CARTESIAN_POINT('',(0.,0.,0.));
#8216=CARTESIAN_POINT('Origin',(0.,0.067277284513851,0.));
#8217=CARTESIAN_POINT('',(-0.375277674973257,0.0768195421087395,0.65));
#8218=CARTESIAN_POINT('',(0.375277674973257,0.0768195421087395,0.65));
#8219=CARTESIAN_POINT('Ctrl Pts',(-0.375277674973257,0.0768195421087395,
0.65));
#8220=CARTESIAN_POINT('Ctrl Pts',(1.66533453693773E-13,-0.0315137912242439,
0.65));
#8221=CARTESIAN_POINT('Ctrl Pts',(0.375277674973257,0.0768195421087394,
0.65));
#8222=CARTESIAN_POINT('',(-0.750555349946514,0.0768195421087394,-9.19165206894919E-17));
#8223=CARTESIAN_POINT('Ctrl Pts',(-0.750555349946514,0.0768195421087394,
-9.19165206894919E-17));
#8224=CARTESIAN_POINT('Ctrl Pts',(-0.562916512459802,-0.0315137912242434,
0.325000000000144));
#8225=CARTESIAN_POINT('Ctrl Pts',(-0.375277674973257,0.0768195421087395,
0.65));
#8226=CARTESIAN_POINT('',(-0.6175,-2.77555756156289E-17,-7.5621939847349E-17));
#8227=CARTESIAN_POINT('',(-0.734027674973257,0.067277284513851,-8.98924642641573E-17));
#8228=CARTESIAN_POINT('Origin',(0.,0.,0.));
#8229=CARTESIAN_POINT('',(-0.375277674973257,0.0768195421087395,-0.65));
#8230=CARTESIAN_POINT('Ctrl Pts',(-0.375277674973257,0.0768195421087395,
-0.65));
#8231=CARTESIAN_POINT('Ctrl Pts',(-0.562916512459968,-0.0315137912242437,
-0.324999999999856));
#8232=CARTESIAN_POINT('Ctrl Pts',(-0.750555349946514,0.0768195421087395,
-9.19165206894919E-17));
#8233=CARTESIAN_POINT('',(0.375277674973257,0.0768195421087395,-0.65));
#8234=CARTESIAN_POINT('Ctrl Pts',(0.375277674973257,0.0768195421087395,
-0.65));
#8235=CARTESIAN_POINT('Ctrl Pts',(-1.66144875635155E-13,-0.0315137912242437,
-0.65));
#8236=CARTESIAN_POINT('Ctrl Pts',(-0.375277674973257,0.0768195421087395,
-0.65));
#8237=CARTESIAN_POINT('',(0.750555349946514,0.0768195421087394,0.));
#8238=CARTESIAN_POINT('Ctrl Pts',(0.750555349946514,0.0768195421087394,
0.));
#8239=CARTESIAN_POINT('Ctrl Pts',(0.562916512459802,-0.0315137912242436,
-0.325000000000144));
#8240=CARTESIAN_POINT('Ctrl Pts',(0.375277674973257,0.0768195421087395,
-0.65));
#8241=CARTESIAN_POINT('Ctrl Pts',(0.375277674973257,0.0768195421087394,
0.65));
#8242=CARTESIAN_POINT('Ctrl Pts',(0.562916512459968,-0.0315137912242439,
0.324999999999856));
#8243=CARTESIAN_POINT('Ctrl Pts',(0.750555349946514,0.0768195421087394,
0.));
#8244=CARTESIAN_POINT('Origin',(0.,0.612722715486149,0.));
#8245=CARTESIAN_POINT('',(-0.6175,0.68,-7.5621939847349E-17));
#8246=CARTESIAN_POINT('Origin',(0.,0.68,0.));
#8247=CARTESIAN_POINT('',(-0.750555349946514,0.603180457891261,-9.19165206894919E-17));
#8248=CARTESIAN_POINT('',(-0.734027674973257,0.612722715486149,-8.98924642641573E-17));
#8249=CARTESIAN_POINT('',(-0.375277674973257,0.603180457891261,0.65));
#8250=CARTESIAN_POINT('Ctrl Pts',(-0.375277674973257,0.603180457891261,
0.65));
#8251=CARTESIAN_POINT('Ctrl Pts',(-0.562916512459968,0.711513791224243,
0.324999999999856));
#8252=CARTESIAN_POINT('Ctrl Pts',(-0.750555349946514,0.603180457891261,
-9.19165206894919E-17));
#8253=CARTESIAN_POINT('',(0.375277674973257,0.603180457891261,0.65));
#8254=CARTESIAN_POINT('Ctrl Pts',(0.375277674973257,0.603180457891261,0.65));
#8255=CARTESIAN_POINT('Ctrl Pts',(-1.66755498298699E-13,0.711513791224244,
0.65));
#8256=CARTESIAN_POINT('Ctrl Pts',(-0.375277674973257,0.603180457891261,
0.65));
#8257=CARTESIAN_POINT('',(0.750555349946514,0.603180457891261,0.));
#8258=CARTESIAN_POINT('Ctrl Pts',(0.750555349946514,0.603180457891261,0.));
#8259=CARTESIAN_POINT('Ctrl Pts',(0.562916512459802,0.711513791224244,0.325000000000144));
#8260=CARTESIAN_POINT('Ctrl Pts',(0.375277674973257,0.603180457891261,0.65));
#8261=CARTESIAN_POINT('',(0.375277674973257,0.603180457891261,-0.65));
#8262=CARTESIAN_POINT('Ctrl Pts',(0.375277674973257,0.603180457891261,-0.65));
#8263=CARTESIAN_POINT('Ctrl Pts',(0.562916512459969,0.711513791224244,-0.324999999999856));
#8264=CARTESIAN_POINT('Ctrl Pts',(0.750555349946514,0.603180457891261,0.));
#8265=CARTESIAN_POINT('',(-0.375277674973257,0.603180457891261,-0.65));
#8266=CARTESIAN_POINT('Ctrl Pts',(-0.375277674973257,0.603180457891261,
-0.65));
#8267=CARTESIAN_POINT('Ctrl Pts',(1.66422431391311E-13,0.711513791224244,
-0.65));
#8268=CARTESIAN_POINT('Ctrl Pts',(0.375277674973257,0.603180457891261,-0.65));
#8269=CARTESIAN_POINT('Ctrl Pts',(-0.750555349946514,0.603180457891261,
-9.19165206894919E-17));
#8270=CARTESIAN_POINT('Ctrl Pts',(-0.562916512459802,0.711513791224244,
-0.325000000000144));
#8271=CARTESIAN_POINT('Ctrl Pts',(-0.375277674973257,0.603180457891261,
-0.65));
#8272=CARTESIAN_POINT('Origin',(0.375277674973257,0.,-0.65));
#8273=CARTESIAN_POINT('',(-0.375277674973257,0.,-0.65));
#8274=CARTESIAN_POINT('',(0.375277674973257,0.,-0.65));
#8275=CARTESIAN_POINT('Origin',(-0.375277674973257,0.,-0.65));
#8276=CARTESIAN_POINT('',(-0.750555349946514,0.,-9.19165206894919E-17));
#8277=CARTESIAN_POINT('Origin',(-0.750555349946514,0.,-9.19165206894919E-17));
#8278=CARTESIAN_POINT('',(-0.375277674973257,0.,0.65));
#8279=CARTESIAN_POINT('Origin',(0.,0.,0.));
#8280=CARTESIAN_POINT('',(-0.338975,0.68,4.15124648740974E-17));
#8281=CARTESIAN_POINT('Origin',(0.,0.68,0.));
#8282=CARTESIAN_POINT('',(-0.338975,0.,4.15124648740974E-17));
#8283=CARTESIAN_POINT('',(-0.338975,0.,4.15124648740974E-17));
#8284=CARTESIAN_POINT('Origin',(0.,0.,0.));
#8285=CARTESIAN_POINT('Origin',(-0.375277674973257,0.,0.65));
#8286=CARTESIAN_POINT('',(0.375277674973257,0.,0.65));
#8287=CARTESIAN_POINT('Origin',(0.750555349946514,0.,0.));
#8288=CARTESIAN_POINT('',(0.750555349946514,0.,0.));
#8289=CARTESIAN_POINT('Origin',(0.375277674973257,0.,0.65));
#8290=CARTESIAN_POINT('Origin',(0.,0.68,-1.11022302462516E-16));
#8291=CARTESIAN_POINT('Origin',(0.,0.,-1.11022302462516E-16));
#8292=CARTESIAN_POINT('',(0.,0.,0.));
#8293=CARTESIAN_POINT('Origin',(0.0577350269189626,0.,-0.1));
#8294=CARTESIAN_POINT('',(0.0577350269189626,0.,-0.1));
#8295=CARTESIAN_POINT('',(0.115470053837925,0.,0.));
#8296=CARTESIAN_POINT('',(0.0934187836487032,0.,-0.0381939203391614));
#8297=CARTESIAN_POINT('',(0.0577350269189626,-0.2,-0.1));
#8298=CARTESIAN_POINT('',(0.0577350269189626,0.,-0.1));
#8299=CARTESIAN_POINT('',(0.115470053837925,-0.2,0.));
#8300=CARTESIAN_POINT('',(0.115470053837925,-0.2,0.));
#8301=CARTESIAN_POINT('',(0.115470053837925,0.,0.));
#8302=CARTESIAN_POINT('Origin',(-0.0577350269189626,0.,-0.1));
#8303=CARTESIAN_POINT('',(-0.0577350269189626,0.,-0.1));
#8304=CARTESIAN_POINT('',(0.0561324865405187,0.,-0.1));
#8305=CARTESIAN_POINT('',(-0.0577350269189626,-0.2,-0.1));
#8306=CARTESIAN_POINT('',(-0.0577350269189626,0.,-0.1));
#8307=CARTESIAN_POINT('',(0.0577350269189626,-0.2,-0.1));
#8308=CARTESIAN_POINT('Origin',(-0.115470053837925,0.,-1.38777878078145E-17));
#8309=CARTESIAN_POINT('',(-0.115470053837925,0.,-1.41410031829988E-17));
#8310=CARTESIAN_POINT('',(-0.0797862971081845,0.,-0.0618060796608387));
#8311=CARTESIAN_POINT('',(-0.115470053837925,-0.2,-1.38777878078145E-17));
#8312=CARTESIAN_POINT('',(-0.115470053837925,0.,-1.41410031829988E-17));
#8313=CARTESIAN_POINT('',(-0.0577350269189626,-0.2,-0.1));
#8314=CARTESIAN_POINT('Origin',(-0.0577350269189626,0.,0.1));
#8315=CARTESIAN_POINT('',(-0.0577350269189626,0.,0.1));
#8316=CARTESIAN_POINT('',(-0.0509187836487033,0.,0.111806079660839));
#8317=CARTESIAN_POINT('',(-0.0577350269189626,-0.2,0.1));
#8318=CARTESIAN_POINT('',(-0.0577350269189626,0.,0.1));
#8319=CARTESIAN_POINT('',(-0.115470053837925,-0.2,-1.41410031829988E-17));
#8320=CARTESIAN_POINT('Origin',(0.0577350269189626,0.,0.1));
#8321=CARTESIAN_POINT('',(0.0577350269189626,0.,0.1));
#8322=CARTESIAN_POINT('',(0.113867513459481,0.,0.1));
#8323=CARTESIAN_POINT('',(0.0577350269189626,-0.2,0.1));
#8324=CARTESIAN_POINT('',(0.0577350269189626,0.,0.1));
#8325=CARTESIAN_POINT('',(-0.0577350269189626,-0.2,0.1));
#8326=CARTESIAN_POINT('Origin',(0.115470053837925,0.,0.));
#8327=CARTESIAN_POINT('',(0.122286297108185,0.,-0.0118060796608386));
#8328=CARTESIAN_POINT('',(0.0577350269189626,-0.2,0.1));
#8329=CARTESIAN_POINT('Origin',(0.,-0.2,0.));
#8330=CARTESIAN_POINT('Origin',(0.17,0.,0.));
#8331=CARTESIAN_POINT('',(-0.17,-8.67361737988404E-18,-2.0818995585505E-17));
#8332=CARTESIAN_POINT('Origin',(0.,0.,0.));
#8333=CARTESIAN_POINT('Origin',(0.,-0.015,0.));
#8334=CARTESIAN_POINT('',(-0.1954,-0.0254,-2.39295984553393E-17));
#8335=CARTESIAN_POINT('Origin',(0.,-0.0254,0.));
#8336=CARTESIAN_POINT('',(-0.185,-0.015,-2.2655965784226E-17));
#8337=CARTESIAN_POINT('Origin',(0.,-0.2775,0.));
#8338=CARTESIAN_POINT('',(-0.1954,-0.5296,2.39295984553393E-17));
#8339=CARTESIAN_POINT('Origin',(0.,-0.5296,0.));
#8340=CARTESIAN_POINT('',(-0.1954,-0.2775,-2.39295984553393E-17));
#8341=CARTESIAN_POINT('Origin',(0.,-0.5625,0.));
#8342=CARTESIAN_POINT('',(-0.125,-0.6,-1.53080849893419E-17));
#8343=CARTESIAN_POINT('Origin',(0.,-0.6,0.));
#8344=CARTESIAN_POINT('',(-0.1625,-0.5625,-1.99005104861445E-17));
#8345=CARTESIAN_POINT('Origin',(0.,-0.6,0.));
#8346=CARTESIAN_POINT('',(0.,0.,0.));
#8347=CARTESIAN_POINT('',(0.,0.,0.));
#8348=CARTESIAN_POINT('',(0.,0.,0.));
#8349=CARTESIAN_POINT('',(0.,0.,0.));
#8350=CARTESIAN_POINT('',(0.,0.,0.));
#8351=CARTESIAN_POINT('',(0.,0.,0.));
#8352=CARTESIAN_POINT('',(0.,0.,0.));
#8353=CARTESIAN_POINT('',(0.,0.,0.));
#8354=CARTESIAN_POINT('',(0.,0.,0.));
#8355=CARTESIAN_POINT('',(0.,0.,0.));
#8356=CARTESIAN_POINT('',(0.,0.,0.));
#8357=CARTESIAN_POINT('',(0.,0.,0.));
#8358=CARTESIAN_POINT('',(0.,0.,0.));
#8359=CARTESIAN_POINT('',(0.,0.,0.));
#8360=CARTESIAN_POINT('',(0.,0.,0.));
#8361=CARTESIAN_POINT('',(0.,0.,0.));
#8362=CARTESIAN_POINT('',(0.,0.,0.));
#8363=CARTESIAN_POINT('',(0.,0.,0.));
#8364=CARTESIAN_POINT('',(0.,-3.,0.));
#8365=CARTESIAN_POINT('',(0.,3.,0.));
#8366=CARTESIAN_POINT('',(-4.5,0.,1.9));
#8367=CARTESIAN_POINT('',(4.5,0.,3.9));
#8368=CARTESIAN_POINT('',(2.94448637286709,1.7,5.7));
#8369=CARTESIAN_POINT('',(0.,3.4,5.7));
#8370=CARTESIAN_POINT('',(-2.94448637286709,1.7,5.7));
#8371=CARTESIAN_POINT('',(-2.94448637286709,-1.7,5.7));
#8372=CARTESIAN_POINT('',(-4.44089209850063E-16,-3.4,5.7));
#8373=CARTESIAN_POINT('',(2.94448637286709,-1.7,5.7));
#8374=CARTESIAN_POINT('',(0.,0.,9.5));
#8375=CARTESIAN_POINT('',(0.,0.,9.66));
#8376=CARTESIAN_POINT('',(0.,1.,11.));
#8377=UNCERTAINTY_MEASURE_WITH_UNIT(LENGTH_MEASURE(0.001),#8429,
'DISTANCE_ACCURACY_VALUE',
'Maximum model space distance between geometric entities at asserted c
onnectivities');
#8378=UNCERTAINTY_MEASURE_WITH_UNIT(LENGTH_MEASURE(0.001),#8429,
'DISTANCE_ACCURACY_VALUE',
'Maximum model space distance between geometric entities at asserted c
onnectivities');
#8379=UNCERTAINTY_MEASURE_WITH_UNIT(LENGTH_MEASURE(0.001),#8429,
'DISTANCE_ACCURACY_VALUE',
'Maximum model space distance between geometric entities at asserted c
onnectivities');
#8380=UNCERTAINTY_MEASURE_WITH_UNIT(LENGTH_MEASURE(0.001),#8429,
'DISTANCE_ACCURACY_VALUE',
'Maximum model space distance between geometric entities at asserted c
onnectivities');
#8381=UNCERTAINTY_MEASURE_WITH_UNIT(LENGTH_MEASURE(0.001),#8429,
'DISTANCE_ACCURACY_VALUE',
'Maximum model space distance between geometric entities at asserted c
onnectivities');
#8382=UNCERTAINTY_MEASURE_WITH_UNIT(LENGTH_MEASURE(0.001),#8429,
'DISTANCE_ACCURACY_VALUE',
'Maximum model space distance between geometric entities at asserted c
onnectivities');
#8383=UNCERTAINTY_MEASURE_WITH_UNIT(LENGTH_MEASURE(0.001),#8429,
'DISTANCE_ACCURACY_VALUE',
'Maximum model space distance between geometric entities at asserted c
onnectivities');
#8384=UNCERTAINTY_MEASURE_WITH_UNIT(LENGTH_MEASURE(0.001),#8429,
'DISTANCE_ACCURACY_VALUE',
'Maximum model space distance between geometric entities at asserted c
onnectivities');
#8385=UNCERTAINTY_MEASURE_WITH_UNIT(LENGTH_MEASURE(0.001),#8429,
'DISTANCE_ACCURACY_VALUE',
'Maximum model space distance between geometric entities at asserted c
onnectivities');
#8386=UNCERTAINTY_MEASURE_WITH_UNIT(LENGTH_MEASURE(0.001),#8429,
'DISTANCE_ACCURACY_VALUE',
'Maximum model space distance between geometric entities at asserted c
onnectivities');
#8387=UNCERTAINTY_MEASURE_WITH_UNIT(LENGTH_MEASURE(0.001),#8429,
'DISTANCE_ACCURACY_VALUE',
'Maximum model space distance between geometric entities at asserted c
onnectivities');
#8388=UNCERTAINTY_MEASURE_WITH_UNIT(LENGTH_MEASURE(0.001),#8429,
'DISTANCE_ACCURACY_VALUE',
'Maximum model space distance between geometric entities at asserted c
onnectivities');
#8389=UNCERTAINTY_MEASURE_WITH_UNIT(LENGTH_MEASURE(0.001),#8429,
'DISTANCE_ACCURACY_VALUE',
'Maximum model space distance between geometric entities at asserted c
onnectivities');
#8390=UNCERTAINTY_MEASURE_WITH_UNIT(LENGTH_MEASURE(0.001),#8429,
'DISTANCE_ACCURACY_VALUE',
'Maximum model space distance between geometric entities at asserted c
onnectivities');
#8391=UNCERTAINTY_MEASURE_WITH_UNIT(LENGTH_MEASURE(0.001),#8429,
'DISTANCE_ACCURACY_VALUE',
'Maximum model space distance between geometric entities at asserted c
onnectivities');
#8392=UNCERTAINTY_MEASURE_WITH_UNIT(LENGTH_MEASURE(0.001),#8429,
'DISTANCE_ACCURACY_VALUE',
'Maximum model space distance between geometric entities at asserted c
onnectivities');
#8393=UNCERTAINTY_MEASURE_WITH_UNIT(LENGTH_MEASURE(0.001),#8429,
'DISTANCE_ACCURACY_VALUE',
'Maximum model space distance between geometric entities at asserted c
onnectivities');
#8394=UNCERTAINTY_MEASURE_WITH_UNIT(LENGTH_MEASURE(0.001),#8429,
'DISTANCE_ACCURACY_VALUE',
'Maximum model space distance between geometric entities at asserted c
onnectivities');
#8395=UNCERTAINTY_MEASURE_WITH_UNIT(LENGTH_MEASURE(0.001),#8429,
'DISTANCE_ACCURACY_VALUE',
'Maximum model space distance between geometric entities at asserted c
onnectivities');
#8396=UNCERTAINTY_MEASURE_WITH_UNIT(LENGTH_MEASURE(0.001),#8429,
'DISTANCE_ACCURACY_VALUE',
'Maximum model space distance between geometric entities at asserted c
onnectivities');
#8397=UNCERTAINTY_MEASURE_WITH_UNIT(LENGTH_MEASURE(0.001),#8429,
'DISTANCE_ACCURACY_VALUE',
'Maximum model space distance between geometric entities at asserted c
onnectivities');
#8398=UNCERTAINTY_MEASURE_WITH_UNIT(LENGTH_MEASURE(0.001),#8429,
'DISTANCE_ACCURACY_VALUE',
'Maximum model space distance between geometric entities at asserted c
onnectivities');
#8399=UNCERTAINTY_MEASURE_WITH_UNIT(LENGTH_MEASURE(0.001),#8429,
'DISTANCE_ACCURACY_VALUE',
'Maximum model space distance between geometric entities at asserted c
onnectivities');
#8400=UNCERTAINTY_MEASURE_WITH_UNIT(LENGTH_MEASURE(0.001),#8429,
'DISTANCE_ACCURACY_VALUE',
'Maximum model space distance between geometric entities at asserted c
onnectivities');
#8401=UNCERTAINTY_MEASURE_WITH_UNIT(LENGTH_MEASURE(0.001),#8429,
'DISTANCE_ACCURACY_VALUE',
'Maximum model space distance between geometric entities at asserted c
onnectivities');
#8402=UNCERTAINTY_MEASURE_WITH_UNIT(LENGTH_MEASURE(0.001),#8429,
'DISTANCE_ACCURACY_VALUE',
'Maximum model space distance between geometric entities at asserted c
onnectivities');
#8403=(
GEOMETRIC_REPRESENTATION_CONTEXT(3)
GLOBAL_UNCERTAINTY_ASSIGNED_CONTEXT((#8377))
GLOBAL_UNIT_ASSIGNED_CONTEXT((#8429,#8431,#8432))
REPRESENTATION_CONTEXT('','3D')
);
#8404=(
GEOMETRIC_REPRESENTATION_CONTEXT(3)
GLOBAL_UNCERTAINTY_ASSIGNED_CONTEXT((#8378))
GLOBAL_UNIT_ASSIGNED_CONTEXT((#8429,#8431,#8432))
REPRESENTATION_CONTEXT('','3D')
);
#8405=(
GEOMETRIC_REPRESENTATION_CONTEXT(3)
GLOBAL_UNCERTAINTY_ASSIGNED_CONTEXT((#8379))
GLOBAL_UNIT_ASSIGNED_CONTEXT((#8429,#8431,#8432))
REPRESENTATION_CONTEXT('','3D')
);
#8406=(
GEOMETRIC_REPRESENTATION_CONTEXT(3)
GLOBAL_UNCERTAINTY_ASSIGNED_CONTEXT((#8380))
GLOBAL_UNIT_ASSIGNED_CONTEXT((#8429,#8431,#8432))
REPRESENTATION_CONTEXT('','3D')
);
#8407=(
GEOMETRIC_REPRESENTATION_CONTEXT(3)
GLOBAL_UNCERTAINTY_ASSIGNED_CONTEXT((#8381))
GLOBAL_UNIT_ASSIGNED_CONTEXT((#8429,#8431,#8432))
REPRESENTATION_CONTEXT('','3D')
);
#8408=(
GEOMETRIC_REPRESENTATION_CONTEXT(3)
GLOBAL_UNCERTAINTY_ASSIGNED_CONTEXT((#8382))
GLOBAL_UNIT_ASSIGNED_CONTEXT((#8429,#8431,#8432))
REPRESENTATION_CONTEXT('','3D')
);
#8409=(
GEOMETRIC_REPRESENTATION_CONTEXT(3)
GLOBAL_UNCERTAINTY_ASSIGNED_CONTEXT((#8383))
GLOBAL_UNIT_ASSIGNED_CONTEXT((#8429,#8431,#8432))
REPRESENTATION_CONTEXT('','3D')
);
#8410=(
GEOMETRIC_REPRESENTATION_CONTEXT(3)
GLOBAL_UNCERTAINTY_ASSIGNED_CONTEXT((#8384))
GLOBAL_UNIT_ASSIGNED_CONTEXT((#8429,#8431,#8432))
REPRESENTATION_CONTEXT('','3D')
);
#8411=(
GEOMETRIC_REPRESENTATION_CONTEXT(3)
GLOBAL_UNCERTAINTY_ASSIGNED_CONTEXT((#8385))
GLOBAL_UNIT_ASSIGNED_CONTEXT((#8429,#8431,#8432))
REPRESENTATION_CONTEXT('','3D')
);
#8412=(
GEOMETRIC_REPRESENTATION_CONTEXT(3)
GLOBAL_UNCERTAINTY_ASSIGNED_CONTEXT((#8386))
GLOBAL_UNIT_ASSIGNED_CONTEXT((#8429,#8431,#8432))
REPRESENTATION_CONTEXT('','3D')
);
#8413=(
GEOMETRIC_REPRESENTATION_CONTEXT(3)
GLOBAL_UNCERTAINTY_ASSIGNED_CONTEXT((#8387))
GLOBAL_UNIT_ASSIGNED_CONTEXT((#8429,#8431,#8432))
REPRESENTATION_CONTEXT('','3D')
);
#8414=(
GEOMETRIC_REPRESENTATION_CONTEXT(3)
GLOBAL_UNCERTAINTY_ASSIGNED_CONTEXT((#8388))
GLOBAL_UNIT_ASSIGNED_CONTEXT((#8429,#8431,#8432))
REPRESENTATION_CONTEXT('','3D')
);
#8415=(
GEOMETRIC_REPRESENTATION_CONTEXT(3)
GLOBAL_UNCERTAINTY_ASSIGNED_CONTEXT((#8389))
GLOBAL_UNIT_ASSIGNED_CONTEXT((#8429,#8431,#8432))
REPRESENTATION_CONTEXT('','3D')
);
#8416=(
GEOMETRIC_REPRESENTATION_CONTEXT(3)
GLOBAL_UNCERTAINTY_ASSIGNED_CONTEXT((#8390))
GLOBAL_UNIT_ASSIGNED_CONTEXT((#8429,#8431,#8432))
REPRESENTATION_CONTEXT('','3D')
);
#8417=(
GEOMETRIC_REPRESENTATION_CONTEXT(3)
GLOBAL_UNCERTAINTY_ASSIGNED_CONTEXT((#8391))
GLOBAL_UNIT_ASSIGNED_CONTEXT((#8429,#8431,#8432))
REPRESENTATION_CONTEXT('','3D')
);
#8418=(
GEOMETRIC_REPRESENTATION_CONTEXT(3)
GLOBAL_UNCERTAINTY_ASSIGNED_CONTEXT((#8392))
GLOBAL_UNIT_ASSIGNED_CONTEXT((#8429,#8431,#8432))
REPRESENTATION_CONTEXT('','3D')
);
#8419=(
GEOMETRIC_REPRESENTATION_CONTEXT(3)
GLOBAL_UNCERTAINTY_ASSIGNED_CONTEXT((#8393))
GLOBAL_UNIT_ASSIGNED_CONTEXT((#8429,#8431,#8432))
REPRESENTATION_CONTEXT('','3D')
);
#8420=(
GEOMETRIC_REPRESENTATION_CONTEXT(3)
GLOBAL_UNCERTAINTY_ASSIGNED_CONTEXT((#8394))
GLOBAL_UNIT_ASSIGNED_CONTEXT((#8429,#8431,#8432))
REPRESENTATION_CONTEXT('','3D')
);
#8421=(
GEOMETRIC_REPRESENTATION_CONTEXT(3)
GLOBAL_UNCERTAINTY_ASSIGNED_CONTEXT((#8395))
GLOBAL_UNIT_ASSIGNED_CONTEXT((#8429,#8431,#8432))
REPRESENTATION_CONTEXT('','3D')
);
#8422=(
GEOMETRIC_REPRESENTATION_CONTEXT(3)
GLOBAL_UNCERTAINTY_ASSIGNED_CONTEXT((#8396))
GLOBAL_UNIT_ASSIGNED_CONTEXT((#8429,#8431,#8432))
REPRESENTATION_CONTEXT('','3D')
);
#8423=(
GEOMETRIC_REPRESENTATION_CONTEXT(3)
GLOBAL_UNCERTAINTY_ASSIGNED_CONTEXT((#8397))
GLOBAL_UNIT_ASSIGNED_CONTEXT((#8429,#8431,#8432))
REPRESENTATION_CONTEXT('','3D')
);
#8424=(
GEOMETRIC_REPRESENTATION_CONTEXT(3)
GLOBAL_UNCERTAINTY_ASSIGNED_CONTEXT((#8398))
GLOBAL_UNIT_ASSIGNED_CONTEXT((#8429,#8431,#8432))
REPRESENTATION_CONTEXT('','3D')
);
#8425=(
GEOMETRIC_REPRESENTATION_CONTEXT(3)
GLOBAL_UNCERTAINTY_ASSIGNED_CONTEXT((#8399))
GLOBAL_UNIT_ASSIGNED_CONTEXT((#8429,#8431,#8432))
REPRESENTATION_CONTEXT('','3D')
);
#8426=(
GEOMETRIC_REPRESENTATION_CONTEXT(3)
GLOBAL_UNCERTAINTY_ASSIGNED_CONTEXT((#8400))
GLOBAL_UNIT_ASSIGNED_CONTEXT((#8429,#8431,#8432))
REPRESENTATION_CONTEXT('','3D')
);
#8427=(
GEOMETRIC_REPRESENTATION_CONTEXT(3)
GLOBAL_UNCERTAINTY_ASSIGNED_CONTEXT((#8401))
GLOBAL_UNIT_ASSIGNED_CONTEXT((#8429,#8431,#8432))
REPRESENTATION_CONTEXT('','3D')
);
#8428=(
GEOMETRIC_REPRESENTATION_CONTEXT(3)
GLOBAL_UNCERTAINTY_ASSIGNED_CONTEXT((#8402))
GLOBAL_UNIT_ASSIGNED_CONTEXT((#8429,#8431,#8432))
REPRESENTATION_CONTEXT('','3D')
);
#8429=(
LENGTH_UNIT()
NAMED_UNIT(*)
SI_UNIT(.CENTI.,.METRE.)
);
#8430=(
LENGTH_UNIT()
NAMED_UNIT(*)
SI_UNIT($,.METRE.)
);
#8431=(
NAMED_UNIT(*)
PLANE_ANGLE_UNIT()
SI_UNIT($,.RADIAN.)
);
#8432=(
NAMED_UNIT(*)
SI_UNIT($,.STERADIAN.)
SOLID_ANGLE_UNIT()
);
#8433=SHAPE_DEFINITION_REPRESENTATION(#8458,#8514);
#8434=SHAPE_DEFINITION_REPRESENTATION(#8459,#8515);
#8435=SHAPE_DEFINITION_REPRESENTATION(#8460,#8516);
#8436=SHAPE_DEFINITION_REPRESENTATION(#8461,#8517);
#8437=SHAPE_DEFINITION_REPRESENTATION(#8462,#8518);
#8438=SHAPE_DEFINITION_REPRESENTATION(#8463,#8519);
#8439=SHAPE_DEFINITION_REPRESENTATION(#8464,#8520);
#8440=SHAPE_DEFINITION_REPRESENTATION(#8465,#8521);
#8441=SHAPE_DEFINITION_REPRESENTATION(#8466,#8522);
#8442=SHAPE_DEFINITION_REPRESENTATION(#8467,#8523);
#8443=SHAPE_DEFINITION_REPRESENTATION(#8468,#8524);
#8444=SHAPE_DEFINITION_REPRESENTATION(#8469,#8525);
#8445=SHAPE_DEFINITION_REPRESENTATION(#8470,#8526);
#8446=SHAPE_DEFINITION_REPRESENTATION(#8471,#8527);
#8447=SHAPE_DEFINITION_REPRESENTATION(#8472,#8528);
#8448=SHAPE_DEFINITION_REPRESENTATION(#8473,#8529);
#8449=SHAPE_DEFINITION_REPRESENTATION(#8474,#8530);
#8450=SHAPE_DEFINITION_REPRESENTATION(#8475,#8531);
#8451=SHAPE_DEFINITION_REPRESENTATION(#8476,#8532);
#8452=SHAPE_DEFINITION_REPRESENTATION(#8477,#8533);
#8453=SHAPE_DEFINITION_REPRESENTATION(#8478,#8534);
#8454=SHAPE_DEFINITION_REPRESENTATION(#8479,#8535);
#8455=SHAPE_DEFINITION_REPRESENTATION(#8480,#8536);
#8456=SHAPE_DEFINITION_REPRESENTATION(#8481,#8537);
#8457=SHAPE_DEFINITION_REPRESENTATION(#8482,#8538);
#8458=PRODUCT_DEFINITION_SHAPE('',$,#8540);
#8459=PRODUCT_DEFINITION_SHAPE('',$,#8541);
#8460=PRODUCT_DEFINITION_SHAPE('',$,#8542);
#8461=PRODUCT_DEFINITION_SHAPE('',$,#8543);
#8462=PRODUCT_DEFINITION_SHAPE('',$,#8544);
#8463=PRODUCT_DEFINITION_SHAPE('',$,#8545);
#8464=PRODUCT_DEFINITION_SHAPE('',$,#8546);
#8465=PRODUCT_DEFINITION_SHAPE('',$,#8547);
#8466=PRODUCT_DEFINITION_SHAPE('',$,#8548);
#8467=PRODUCT_DEFINITION_SHAPE('',$,#8549);
#8468=PRODUCT_DEFINITION_SHAPE('',$,#8550);
#8469=PRODUCT_DEFINITION_SHAPE('',$,#8551);
#8470=PRODUCT_DEFINITION_SHAPE('',$,#8552);
#8471=PRODUCT_DEFINITION_SHAPE('',$,#8553);
#8472=PRODUCT_DEFINITION_SHAPE('',$,#8554);
#8473=PRODUCT_DEFINITION_SHAPE('',$,#8555);
#8474=PRODUCT_DEFINITION_SHAPE('',$,#8556);
#8475=PRODUCT_DEFINITION_SHAPE('',$,#8557);
#8476=PRODUCT_DEFINITION_SHAPE('',$,#8558);
#8477=PRODUCT_DEFINITION_SHAPE('',$,#8559);
#8478=PRODUCT_DEFINITION_SHAPE('',$,#8560);
#8479=PRODUCT_DEFINITION_SHAPE('',$,#8561);
#8480=PRODUCT_DEFINITION_SHAPE('',$,#8562);
#8481=PRODUCT_DEFINITION_SHAPE('',$,#8563);
#8482=PRODUCT_DEFINITION_SHAPE('',$,#8564);
#8483=PRODUCT_DEFINITION_SHAPE($,$,#104);
#8484=PRODUCT_DEFINITION_SHAPE($,$,#105);
#8485=PRODUCT_DEFINITION_SHAPE($,$,#106);
#8486=PRODUCT_DEFINITION_SHAPE($,$,#107);
#8487=PRODUCT_DEFINITION_SHAPE($,$,#108);
#8488=PRODUCT_DEFINITION_SHAPE($,$,#109);
#8489=PRODUCT_DEFINITION_SHAPE($,$,#110);
#8490=PRODUCT_DEFINITION_SHAPE($,$,#111);
#8491=PRODUCT_DEFINITION_SHAPE($,$,#112);
#8492=PRODUCT_DEFINITION_SHAPE($,$,#113);
#8493=PRODUCT_DEFINITION_SHAPE($,$,#114);
#8494=PRODUCT_DEFINITION_SHAPE($,$,#115);
#8495=PRODUCT_DEFINITION_SHAPE($,$,#116);
#8496=PRODUCT_DEFINITION_SHAPE($,$,#117);
#8497=PRODUCT_DEFINITION_SHAPE($,$,#118);
#8498=PRODUCT_DEFINITION_SHAPE($,$,#119);
#8499=PRODUCT_DEFINITION_SHAPE($,$,#120);
#8500=PRODUCT_DEFINITION_SHAPE($,$,#121);
#8501=PRODUCT_DEFINITION_SHAPE($,$,#122);
#8502=PRODUCT_DEFINITION_SHAPE($,$,#123);
#8503=PRODUCT_DEFINITION_SHAPE($,$,#124);
#8504=PRODUCT_DEFINITION_SHAPE($,$,#125);
#8505=PRODUCT_DEFINITION_SHAPE($,$,#126);
#8506=PRODUCT_DEFINITION_SHAPE($,$,#127);
#8507=PRODUCT_DEFINITION_SHAPE($,$,#128);
#8508=PRODUCT_DEFINITION_SHAPE($,$,#129);
#8509=PRODUCT_DEFINITION_SHAPE($,$,#130);
#8510=PRODUCT_DEFINITION_SHAPE($,$,#131);
#8511=PRODUCT_DEFINITION_SHAPE($,$,#132);
#8512=PRODUCT_DEFINITION_SHAPE($,$,#133);
#8513=PRODUCT_DEFINITION_SHAPE($,$,#134);
#8514=SHAPE_REPRESENTATION('',(#3966,#4405,#4406,#4407,#4408,#4409,#4410,
#4411,#4412,#4413,#4414,#4415,#4416,#4417,#4418,#4419,#4420,#4421,#4422,
#4423,#4424,#4425,#4426,#4427,#4428,#4429,#4430,#4431,#4432,#4433,#4434,
#4435),#8403);
#8515=SHAPE_REPRESENTATION('',(#3967),#8404);
#8516=SHAPE_REPRESENTATION('',(#3980),#8405);
#8517=SHAPE_REPRESENTATION('',(#3990),#8406);
#8518=SHAPE_REPRESENTATION('',(#4000),#8407);
#8519=SHAPE_REPRESENTATION('',(#4067),#8408);
#8520=SHAPE_REPRESENTATION('',(#4077),#8409);
#8521=SHAPE_REPRESENTATION('',(#4086),#8410);
#8522=SHAPE_REPRESENTATION('',(#4108),#8411);
#8523=SHAPE_REPRESENTATION('',(#4113),#8412);
#8524=SHAPE_REPRESENTATION('',(#4122),#8413);
#8525=SHAPE_REPRESENTATION('',(#4149),#8414);
#8526=SHAPE_REPRESENTATION('',(#4166),#8415);
#8527=SHAPE_REPRESENTATION('',(#4237),#8416);
#8528=SHAPE_REPRESENTATION('',(#4242),#8417);
#8529=SHAPE_REPRESENTATION('',(#4252),#8418);
#8530=SHAPE_REPRESENTATION('',(#4258),#8419);
#8531=SHAPE_REPRESENTATION('',(#4273),#8420);
#8532=SHAPE_REPRESENTATION('',(#4280),#8421);
#8533=SHAPE_REPRESENTATION('',(#4287),#8422);
#8534=SHAPE_REPRESENTATION('',(#4313),#8423);
#8535=SHAPE_REPRESENTATION('',(#4337),#8424);
#8536=SHAPE_REPRESENTATION('',(#4363),#8425);
#8537=SHAPE_REPRESENTATION('',(#4372),#8426);
#8538=SHAPE_REPRESENTATION('',(#4388),#8427);
#8539=PRODUCT_DEFINITION_CONTEXT('part definition',#8616,'design');
#8540=PRODUCT_DEFINITION('PAT-083','PAT-083',
#8565,#8539);
#8541=PRODUCT_DEFINITION('Base','Base',#8566,#8539);
#8542=PRODUCT_DEFINITION('Mounting foot','Mounting foot',#8567,
#8539);
#8543=PRODUCT_DEFINITION('Mounting foot (1)','Mounting foot (1)',
#8568,#8539);
#8544=PRODUCT_DEFINITION('Lower body','Lower body',#8569,
#8539);
#8545=PRODUCT_DEFINITION('Bottom service plug',
'Bottom service plug',#8570,#8539);
#8546=PRODUCT_DEFINITION('Valve seat','Valve seat',#8571,
#8539);
#8547=PRODUCT_DEFINITION('Poppet and stem','Poppet and stem',#8572,
#8539);
#8548=PRODUCT_DEFINITION('Poppet return spring',
'Poppet return spring',#8573,#8539);
#8549=PRODUCT_DEFINITION('Lower diaphragm plate',
'Lower diaphragm plate',#8574,#8539);
#8550=PRODUCT_DEFINITION('Diaphragm','Diaphragm',#8575,
#8539);
#8551=PRODUCT_DEFINITION('Upper diaphragm plate',
'Upper diaphragm plate',#8576,#8539);
#8552=PRODUCT_DEFINITION('Bonnet','Bonnet',#8577,#8539);
#8553=PRODUCT_DEFINITION('Control spring','Control spring',#8578,
#8539);
#8554=PRODUCT_DEFINITION('Adjuster spring shoe',
'Adjuster spring shoe',#8579,#8539);
#8555=PRODUCT_DEFINITION('Adjusting screw','Adjusting screw',#8580,
#8539);
#8556=PRODUCT_DEFINITION('Adjuster knob','Adjuster knob',#8581,
#8539);
#8557=PRODUCT_DEFINITION('Foot pad','Foot pad',#8582,#8539);
#8558=PRODUCT_DEFINITION('Foot pad (1)','Foot pad (1)',#8583,
#8539);
#8559=PRODUCT_DEFINITION('Cap Screw - M4x16','Cap Screw - M4x16',
#8584,#8539);
#8560=PRODUCT_DEFINITION('Hex Pipe Nipple - 1-4 Inch Tapered Pipe Thread',
'Hex Pipe Nipple - 1-4 Inch Tapered Pipe Thread',#8585,#8539);
#8561=PRODUCT_DEFINITION('Cap Screw - M5x20',
'Cap Screw - M5x20',#8586,#8539);
#8562=PRODUCT_DEFINITION('Flat Washer - M8','Flat Washer - M8',#8587,
#8539);
#8563=PRODUCT_DEFINITION('Hex Nut - M8','Hex Nut - M8',#8588,
#8539);
#8564=PRODUCT_DEFINITION('Socket Set Screw - M4x6',
'Socket Set Screw - M4x6',#8589,#8539);
#8565=PRODUCT_DEFINITION_FORMATION('',$,#8618);
#8566=PRODUCT_DEFINITION_FORMATION('',$,#8619);
#8567=PRODUCT_DEFINITION_FORMATION('',$,#8620);
#8568=PRODUCT_DEFINITION_FORMATION('',$,#8621);
#8569=PRODUCT_DEFINITION_FORMATION('',$,#8622);
#8570=PRODUCT_DEFINITION_FORMATION('',$,#8623);
#8571=PRODUCT_DEFINITION_FORMATION('',$,#8624);
#8572=PRODUCT_DEFINITION_FORMATION('',$,#8625);
#8573=PRODUCT_DEFINITION_FORMATION('',$,#8626);
#8574=PRODUCT_DEFINITION_FORMATION('',$,#8627);
#8575=PRODUCT_DEFINITION_FORMATION('',$,#8628);
#8576=PRODUCT_DEFINITION_FORMATION('',$,#8629);
#8577=PRODUCT_DEFINITION_FORMATION('',$,#8630);
#8578=PRODUCT_DEFINITION_FORMATION('',$,#8631);
#8579=PRODUCT_DEFINITION_FORMATION('',$,#8632);
#8580=PRODUCT_DEFINITION_FORMATION('',$,#8633);
#8581=PRODUCT_DEFINITION_FORMATION('',$,#8634);
#8582=PRODUCT_DEFINITION_FORMATION('',$,#8635);
#8583=PRODUCT_DEFINITION_FORMATION('',$,#8636);
#8584=PRODUCT_DEFINITION_FORMATION('',$,#8637);
#8585=PRODUCT_DEFINITION_FORMATION('',$,#8638);
#8586=PRODUCT_DEFINITION_FORMATION('',$,#8639);
#8587=PRODUCT_DEFINITION_FORMATION('',$,#8640);
#8588=PRODUCT_DEFINITION_FORMATION('',$,#8641);
#8589=PRODUCT_DEFINITION_FORMATION('',$,#8642);
#8590=PRODUCT_RELATED_PRODUCT_CATEGORY('PAT-083',
'PAT-083',(#8618));
#8591=PRODUCT_RELATED_PRODUCT_CATEGORY('Base','Base',(#8619));
#8592=PRODUCT_RELATED_PRODUCT_CATEGORY('Mounting foot','Mounting foot',
(#8620));
#8593=PRODUCT_RELATED_PRODUCT_CATEGORY('Mounting foot (1)',
'Mounting foot (1)',(#8621));
#8594=PRODUCT_RELATED_PRODUCT_CATEGORY('Lower body','Lower body',(#8622));
#8595=PRODUCT_RELATED_PRODUCT_CATEGORY('Bottom service plug',
'Bottom service plug',(#8623));
#8596=PRODUCT_RELATED_PRODUCT_CATEGORY('Valve seat','Valve seat',(#8624));
#8597=PRODUCT_RELATED_PRODUCT_CATEGORY('Poppet and stem',
'Poppet and stem',(#8625));
#8598=PRODUCT_RELATED_PRODUCT_CATEGORY('Poppet return spring',
'Poppet return spring',(#8626));
#8599=PRODUCT_RELATED_PRODUCT_CATEGORY('Lower diaphragm plate',
'Lower diaphragm plate',(#8627));
#8600=PRODUCT_RELATED_PRODUCT_CATEGORY('Diaphragm','Diaphragm',(#8628));
#8601=PRODUCT_RELATED_PRODUCT_CATEGORY('Upper diaphragm plate',
'Upper diaphragm plate',(#8629));
#8602=PRODUCT_RELATED_PRODUCT_CATEGORY('Bonnet','Bonnet',(#8630));
#8603=PRODUCT_RELATED_PRODUCT_CATEGORY('Control spring',
'Control spring',(#8631));
#8604=PRODUCT_RELATED_PRODUCT_CATEGORY('Adjuster spring shoe',
'Adjuster spring shoe',(#8632));
#8605=PRODUCT_RELATED_PRODUCT_CATEGORY('Adjusting screw',
'Adjusting screw',(#8633));
#8606=PRODUCT_RELATED_PRODUCT_CATEGORY('Adjuster knob','Adjuster knob',
(#8634));
#8607=PRODUCT_RELATED_PRODUCT_CATEGORY('Foot pad','Foot pad',(#8635));
#8608=PRODUCT_RELATED_PRODUCT_CATEGORY('Foot pad (1)','Foot pad (1)',(#8636));
#8609=PRODUCT_RELATED_PRODUCT_CATEGORY('Cap Screw - M4x16',
'Cap Screw - M4x16',(#8637));
#8610=PRODUCT_RELATED_PRODUCT_CATEGORY(
'Hex Pipe Nipple - 1-4 Inch Tapered Pipe Thread',
'Hex Pipe Nipple - 1-4 Inch Tapered Pipe Thread',(#8638));
#8611=PRODUCT_RELATED_PRODUCT_CATEGORY('Cap Screw - M5x20',
'Cap Screw - M5x20',(#8639));
#8612=PRODUCT_RELATED_PRODUCT_CATEGORY('Flat Washer - M8',
'Flat Washer - M8',(#8640));
#8613=PRODUCT_RELATED_PRODUCT_CATEGORY('Hex Nut - M8','Hex Nut - M8',(#8641));
#8614=PRODUCT_RELATED_PRODUCT_CATEGORY('Socket Set Screw - M4x6',
'Socket Set Screw - M4x6',(#8642));
#8615=APPLICATION_PROTOCOL_DEFINITION('international standard',
'automotive_design',2009,#8616);
#8616=APPLICATION_CONTEXT(
'Core Data for Automotive Mechanical Design Process');
#8617=PRODUCT_CONTEXT('part definition',#8616,'mechanical');
#8618=PRODUCT('PAT-083','PAT-083',
'PAT-083',(#8617));
#8619=PRODUCT('Base','Base','Base',(#8617));
#8620=PRODUCT('Mounting foot','Mounting foot',
'Mounting foot',(#8617));
#8621=PRODUCT('Mounting foot (1)','Mounting foot (1)',
'Mounting foot (1)',(#8617));
#8622=PRODUCT('Lower body','Lower body','Lower body',(#8617));
#8623=PRODUCT('Bottom service plug','Bottom service plug',
'Bottom service plug',(#8617));
#8624=PRODUCT('Valve seat','Valve seat','Valve seat',(#8617));
#8625=PRODUCT('Poppet and stem','Poppet and stem',
'Poppet and stem',(#8617));
#8626=PRODUCT('Poppet return spring','Poppet return spring',
'Poppet return spring',(#8617));
#8627=PRODUCT('Lower diaphragm plate','Lower diaphragm plate',
'Lower diaphragm plate',(#8617));
#8628=PRODUCT('Diaphragm','Diaphragm','Diaphragm',(#8617));
#8629=PRODUCT('Upper diaphragm plate','Upper diaphragm plate',
'Upper diaphragm plate',(#8617));
#8630=PRODUCT('Bonnet','Bonnet','Bonnet',(#8617));
#8631=PRODUCT('Control spring','Control spring',
'Control spring',(#8617));
#8632=PRODUCT('Adjuster spring shoe','Adjuster spring shoe',
'Adjuster spring shoe',(#8617));
#8633=PRODUCT('Adjusting screw','Adjusting screw',
'Adjusting screw',(#8617));
#8634=PRODUCT('Adjuster knob','Adjuster knob',
'Adjuster knob',(#8617));
#8635=PRODUCT('Foot pad','Foot pad','Foot pad',(#8617));
#8636=PRODUCT('Foot pad (1)','Foot pad (1)','Foot pad (1)',(#8617));
#8637=PRODUCT('Cap Screw - M4x16','Cap Screw - M4x16',
'Cap Screw - M4x16',(#8617));
#8638=PRODUCT('Hex Pipe Nipple - 1-4 Inch Tapered Pipe Thread',
'Hex Pipe Nipple - 1-4 Inch Tapered Pipe Thread',
'Hex Pipe Nipple - 1-4 Inch Tapered Pipe Thread',(#8617));
#8639=PRODUCT('Cap Screw - M5x20','Cap Screw - M5x20',
'Cap Screw - M5x20',(#8617));
#8640=PRODUCT('Flat Washer - M8','Flat Washer - M8',
'Flat Washer - M8',(#8617));
#8641=PRODUCT('Hex Nut - M8','Hex Nut - M8','Hex Nut - M8',
(#8617));
#8642=PRODUCT('Socket Set Screw - M4x6','Socket Set Screw - M4x6',
'Socket Set Screw - M4x6',(#8617));
#8643=PRESENTATION_STYLE_ASSIGNMENT((#8648));
#8644=PRESENTATION_STYLE_ASSIGNMENT((#8649));
#8645=PRESENTATION_STYLE_ASSIGNMENT((#8650));
#8646=PRESENTATION_STYLE_ASSIGNMENT((#8651));
#8647=PRESENTATION_STYLE_ASSIGNMENT((#8652));
#8648=SURFACE_STYLE_USAGE(.BOTH.,#8653);
#8649=SURFACE_STYLE_USAGE(.BOTH.,#8654);
#8650=SURFACE_STYLE_USAGE(.BOTH.,#8655);
#8651=SURFACE_STYLE_USAGE(.BOTH.,#8656);
#8652=SURFACE_STYLE_USAGE(.BOTH.,#8657);
#8653=SURFACE_SIDE_STYLE('',(#8658));
#8654=SURFACE_SIDE_STYLE('',(#8659));
#8655=SURFACE_SIDE_STYLE('',(#8660));
#8656=SURFACE_SIDE_STYLE('',(#8661));
#8657=SURFACE_SIDE_STYLE('',(#8662));
#8658=SURFACE_STYLE_FILL_AREA(#8663);
#8659=SURFACE_STYLE_FILL_AREA(#8664);
#8660=SURFACE_STYLE_FILL_AREA(#8665);
#8661=SURFACE_STYLE_FILL_AREA(#8666);
#8662=SURFACE_STYLE_FILL_AREA(#8667);
#8663=FILL_AREA_STYLE('Steel - Satin',(#8668));
#8664=FILL_AREA_STYLE('CAD Library Painted - Deep blue',(#8669));
#8665=FILL_AREA_STYLE('CAD Library Painted - Engineering blue',(#8670));
#8666=FILL_AREA_STYLE('CAD Library Painted - Steel gray',(#8671));
#8667=FILL_AREA_STYLE('CAD Library Painted - Graphite',(#8672));
#8668=FILL_AREA_STYLE_COLOUR('Steel - Satin',#8673);
#8669=FILL_AREA_STYLE_COLOUR('CAD Library Painted - Deep blue',#8674);
#8670=FILL_AREA_STYLE_COLOUR('CAD Library Painted - Engineering blue',#8675);
#8671=FILL_AREA_STYLE_COLOUR('CAD Library Painted - Steel gray',#8676);
#8672=FILL_AREA_STYLE_COLOUR('CAD Library Painted - Graphite',#8677);
#8673=COLOUR_RGB('Steel - Satin',0.627450980392157,0.627450980392157,0.627450980392157);
#8674=COLOUR_RGB('CAD Library Painted - Deep blue',0.0784313725490196,0.203921568627451,
0.349019607843137);
#8675=COLOUR_RGB('CAD Library Painted - Engineering blue',0.12156862745098,
0.356862745098039,0.6);
#8676=COLOUR_RGB('CAD Library Painted - Steel gray',0.592156862745098,0.631372549019608,
0.67843137254902);
#8677=COLOUR_RGB('CAD Library Painted - Graphite',0.168627450980392,0.192156862745098,
0.231372549019608);
#8678=COLOUR_RGB('Dark Blue',0.08,0.2,0.34);
#8679=FILL_AREA_STYLE_COLOUR('',#8678);
#8680=FILL_AREA_STYLE('',(#8679));
#8681=SURFACE_STYLE_FILL_AREA(#8680);
#8682=SURFACE_SIDE_STYLE('',(#8681));
#8683=SURFACE_STYLE_USAGE(.BOTH.,#8682);
#8684=PRESENTATION_STYLE_ASSIGNMENT((#8683));
#8685=COLOUR_RGB('Light Blue',0.38,0.62,0.78);
#8686=FILL_AREA_STYLE_COLOUR('',#8685);
#8687=FILL_AREA_STYLE('',(#8686));
#8688=SURFACE_STYLE_FILL_AREA(#8687);
#8689=SURFACE_SIDE_STYLE('',(#8688));
#8690=SURFACE_STYLE_USAGE(.BOTH.,#8689);
#8691=PRESENTATION_STYLE_ASSIGNMENT((#8690));
#8692=COLOUR_RGB('Sky Blue',0.24,0.69,0.87);
#8693=FILL_AREA_STYLE_COLOUR('',#8692);
#8694=FILL_AREA_STYLE('',(#8693));
#8695=SURFACE_STYLE_FILL_AREA(#8694);
#8696=SURFACE_SIDE_STYLE('',(#8695));
#8697=SURFACE_STYLE_USAGE(.BOTH.,#8696);
#8698=PRESENTATION_STYLE_ASSIGNMENT((#8697));
#8699=COLOUR_RGB('Grey',0.48,0.52,0.57);
#8700=FILL_AREA_STYLE_COLOUR('',#8699);
#8701=FILL_AREA_STYLE('',(#8700));
#8702=SURFACE_STYLE_FILL_AREA(#8701);
#8703=SURFACE_SIDE_STYLE('',(#8702));
#8704=SURFACE_STYLE_USAGE(.BOTH.,#8703);
#8705=PRESENTATION_STYLE_ASSIGNMENT((#8704));
#8706=COLOUR_RGB('Black',0.12,0.14,0.17);
#8707=FILL_AREA_STYLE_COLOUR('',#8706);
#8708=FILL_AREA_STYLE('',(#8707));
#8709=SURFACE_STYLE_FILL_AREA(#8708);
#8710=SURFACE_SIDE_STYLE('',(#8709));
#8711=SURFACE_STYLE_USAGE(.BOTH.,#8710);
#8712=PRESENTATION_STYLE_ASSIGNMENT((#8711));
#8713=COLOUR_RGB('Off White',0.89,0.88,0.83);
#8714=FILL_AREA_STYLE_COLOUR('',#8713);
#8715=FILL_AREA_STYLE('',(#8714));
#8716=SURFACE_STYLE_FILL_AREA(#8715);
#8717=SURFACE_SIDE_STYLE('',(#8716));
#8718=SURFACE_STYLE_USAGE(.BOTH.,#8717);
#8719=PRESENTATION_STYLE_ASSIGNMENT((#8718));
ENDSEC;
END-ISO-10303-21;
